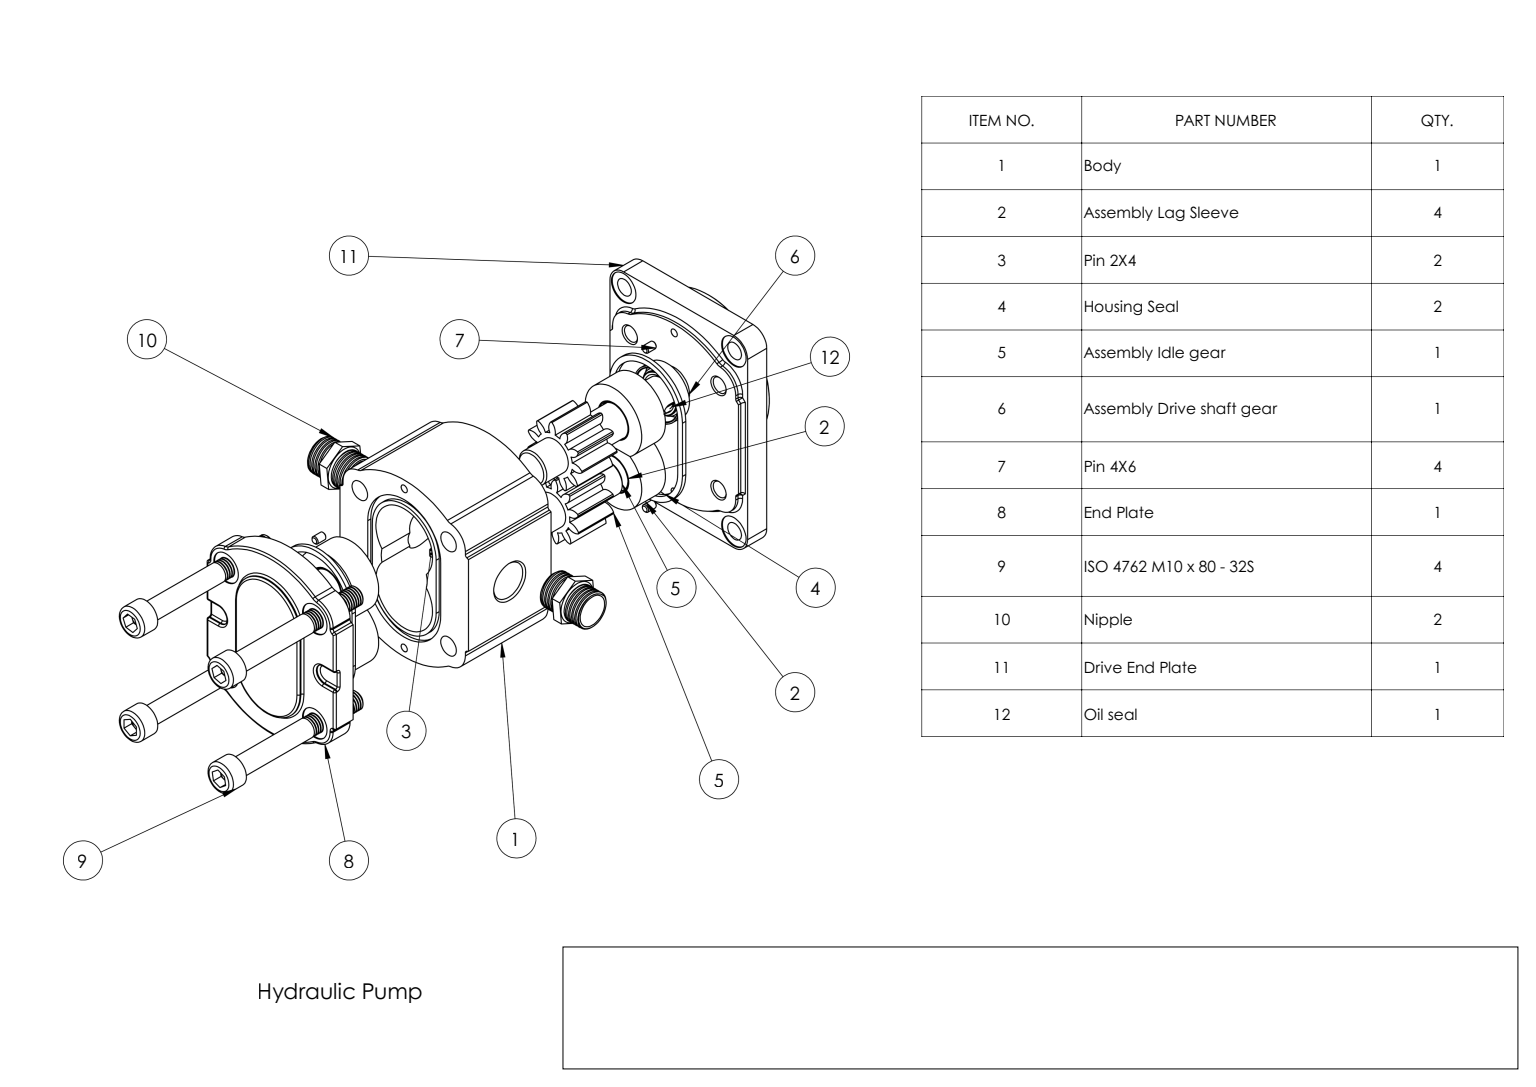
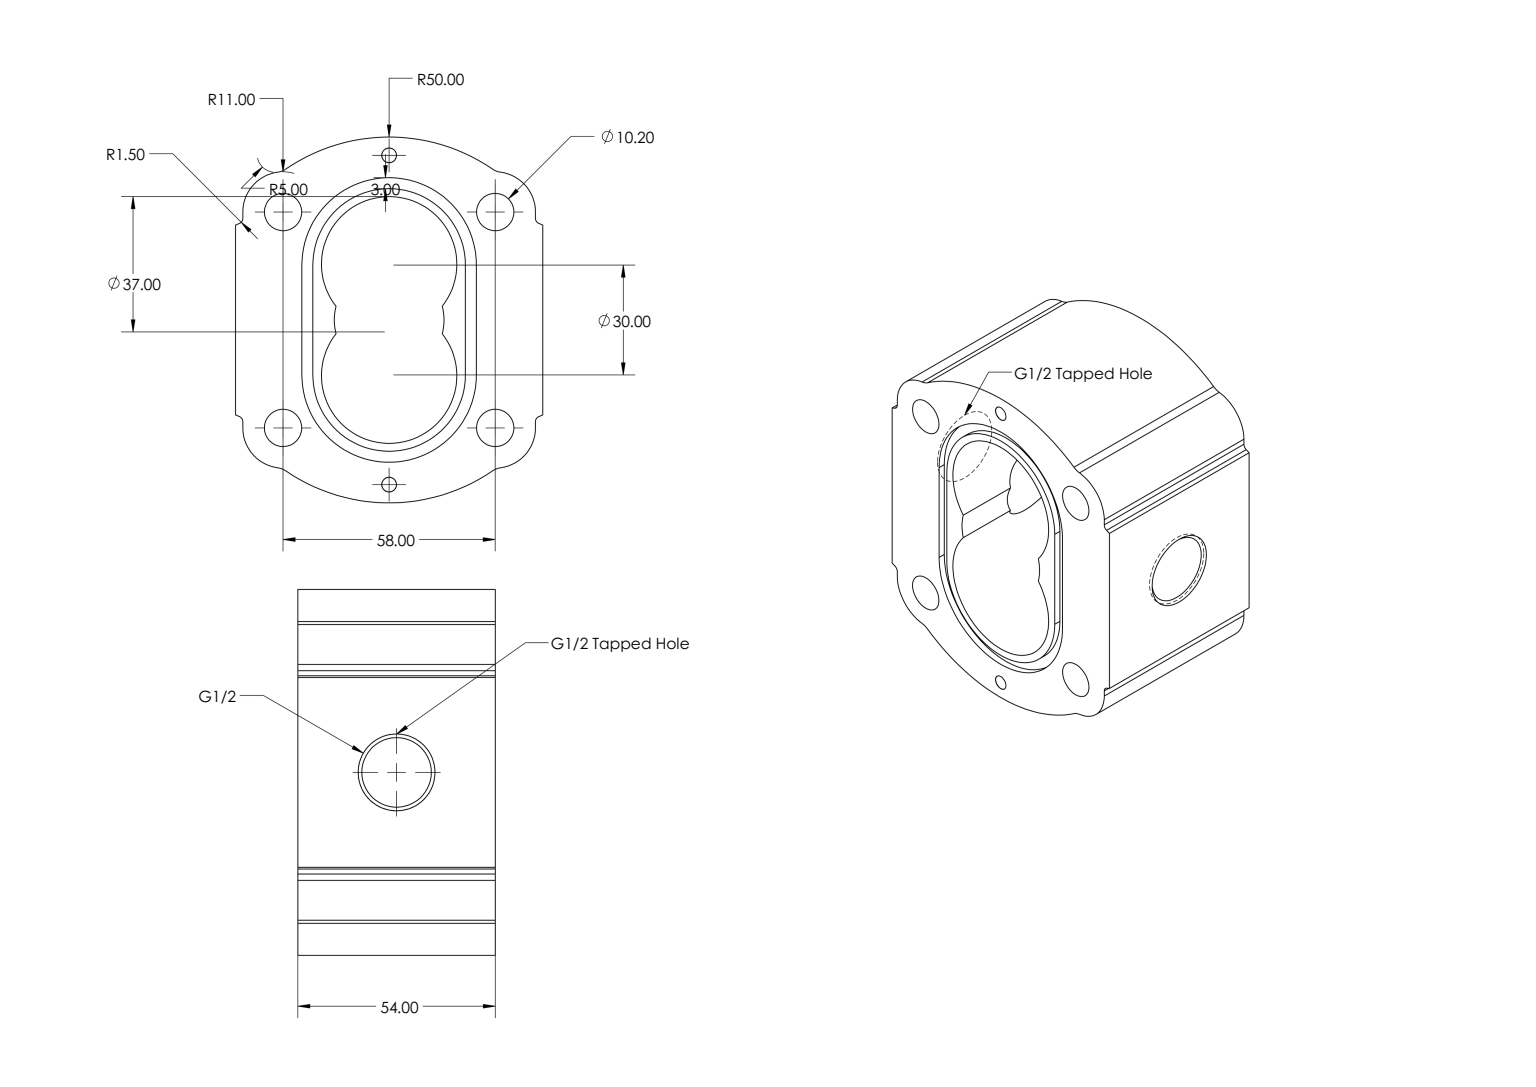
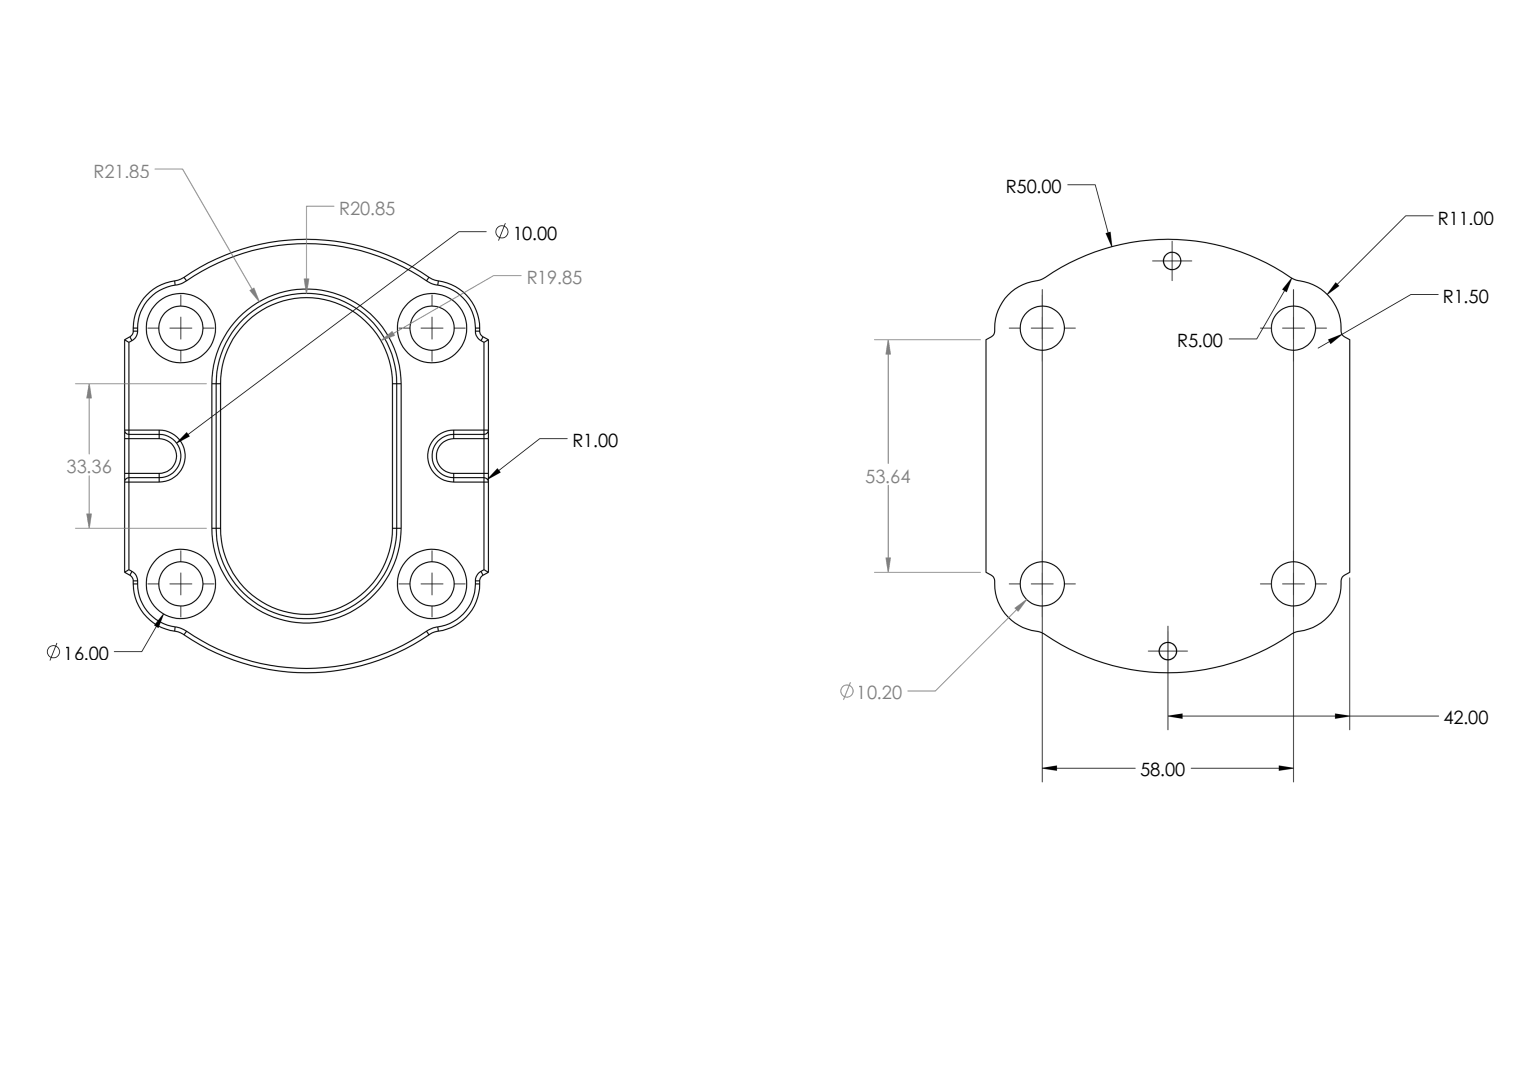
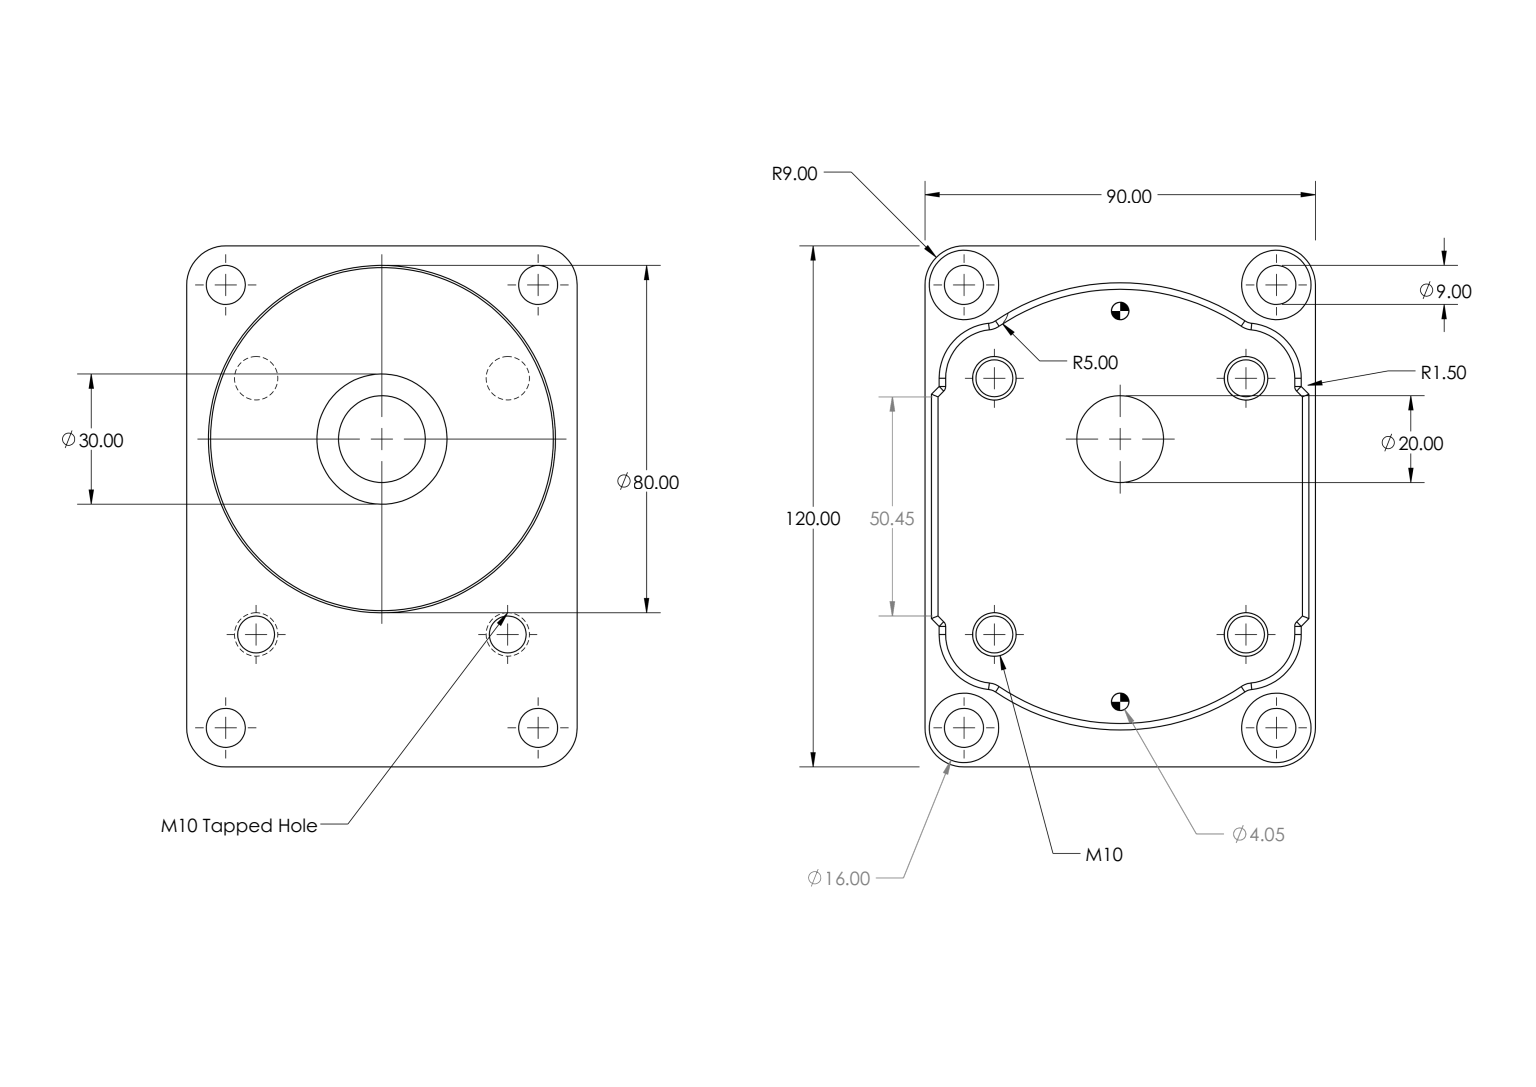
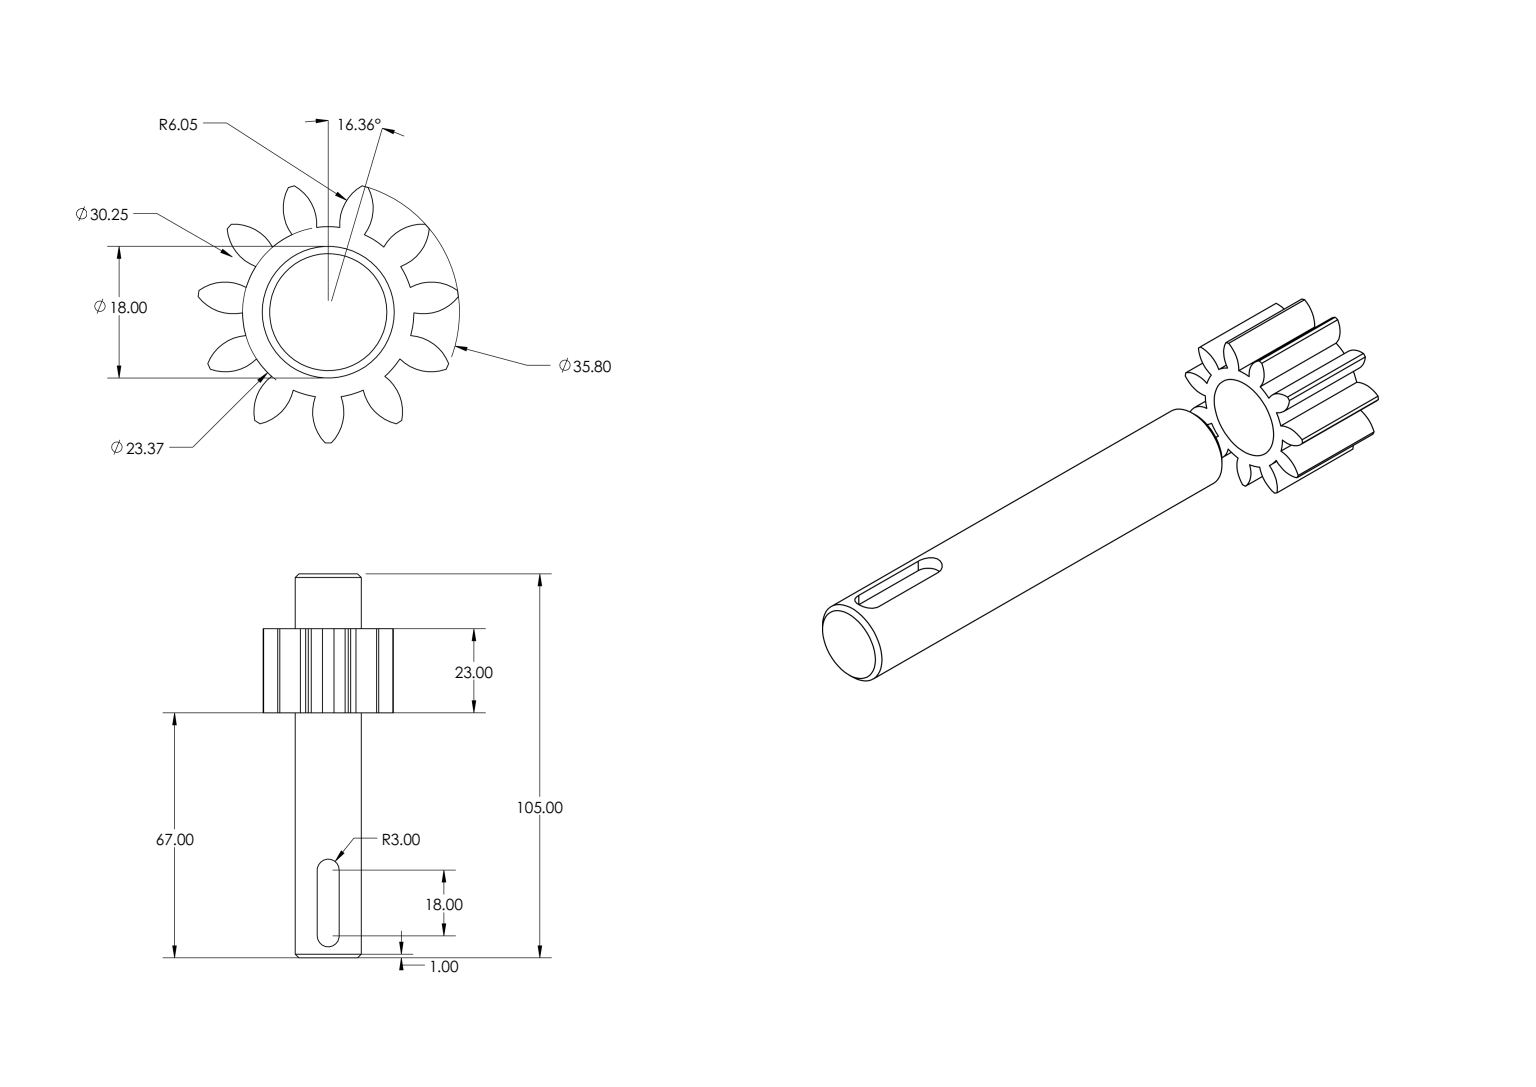
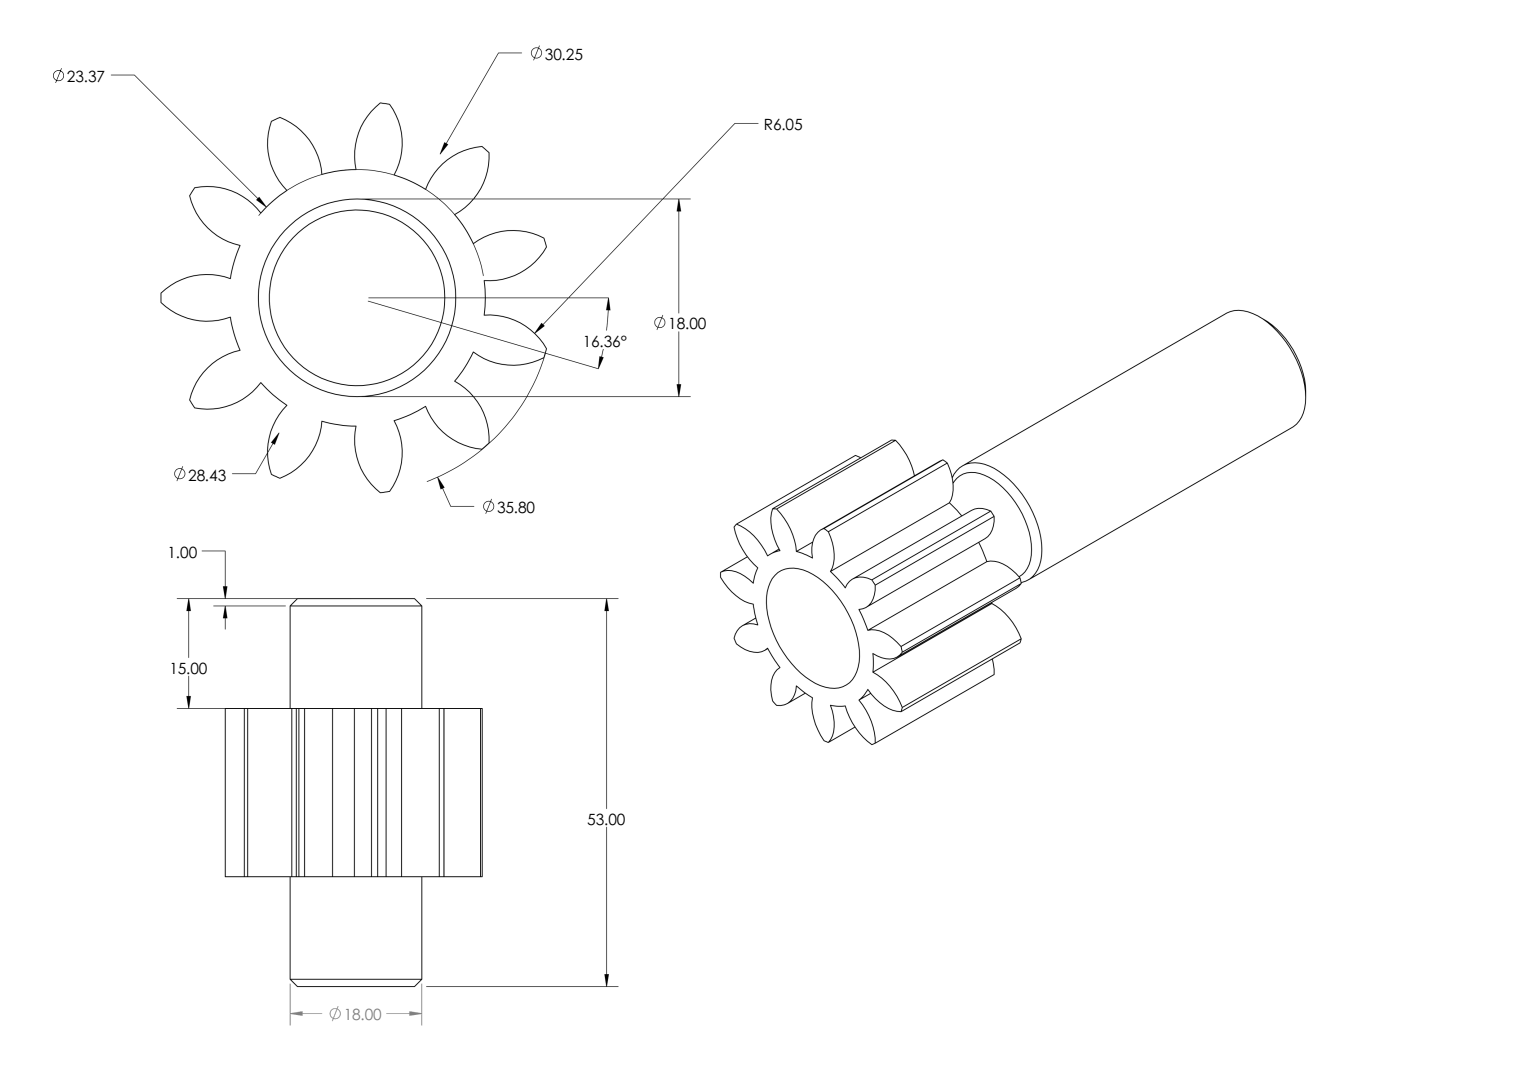
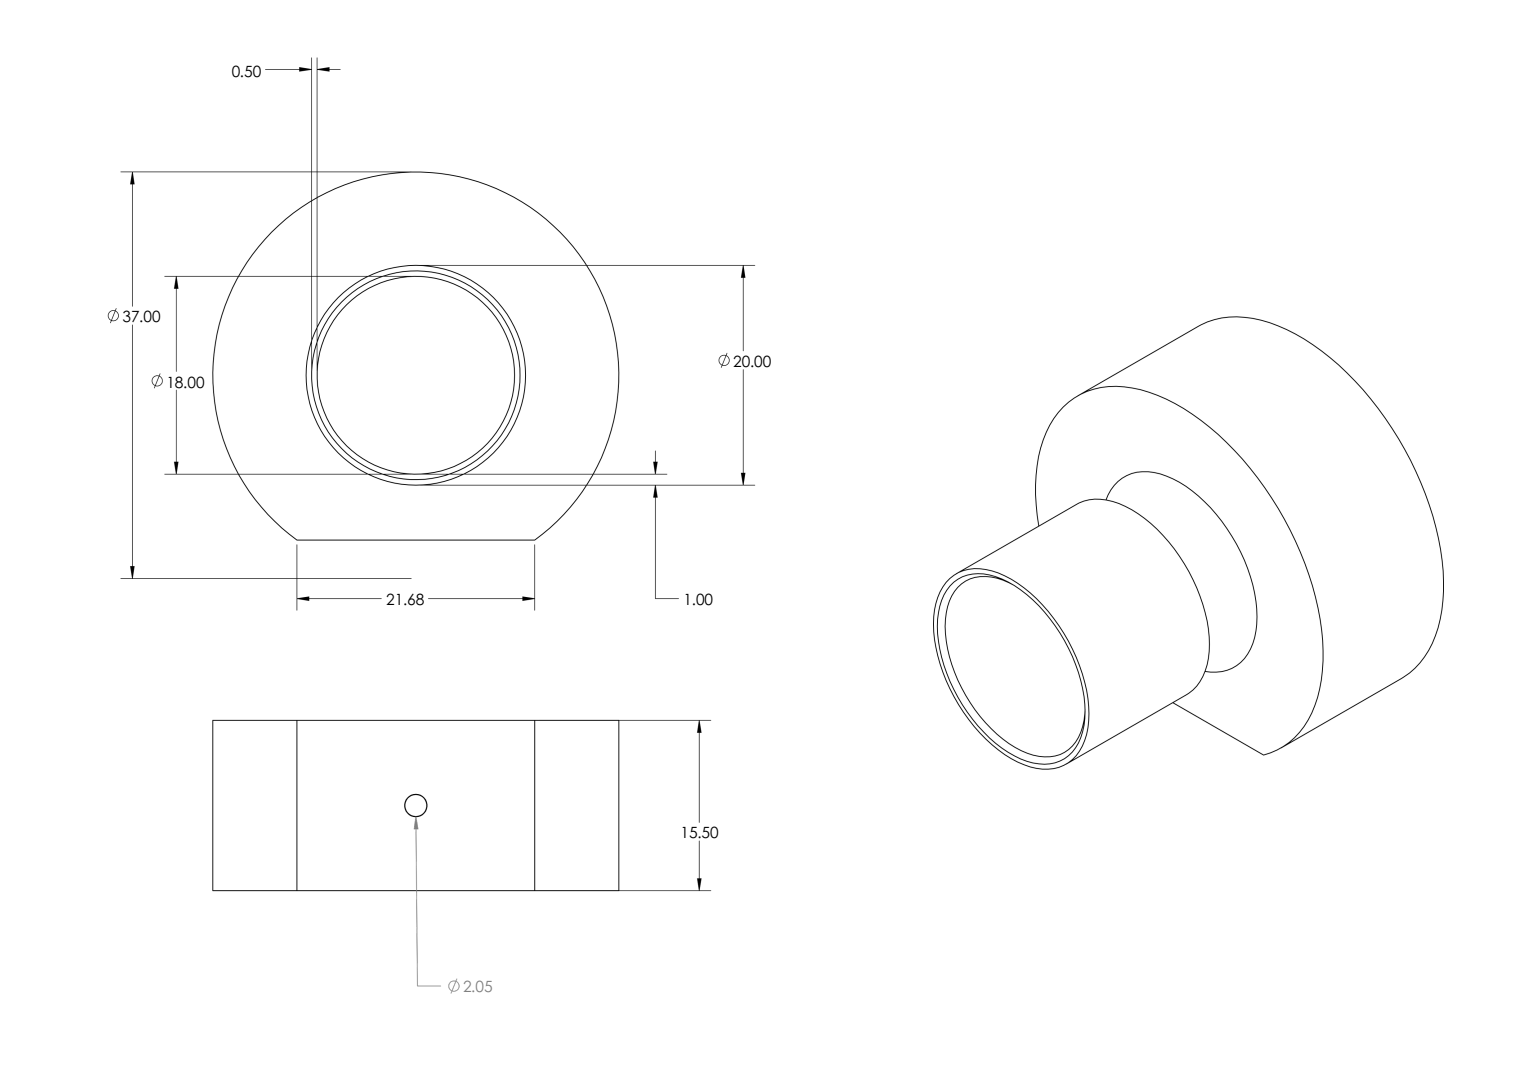
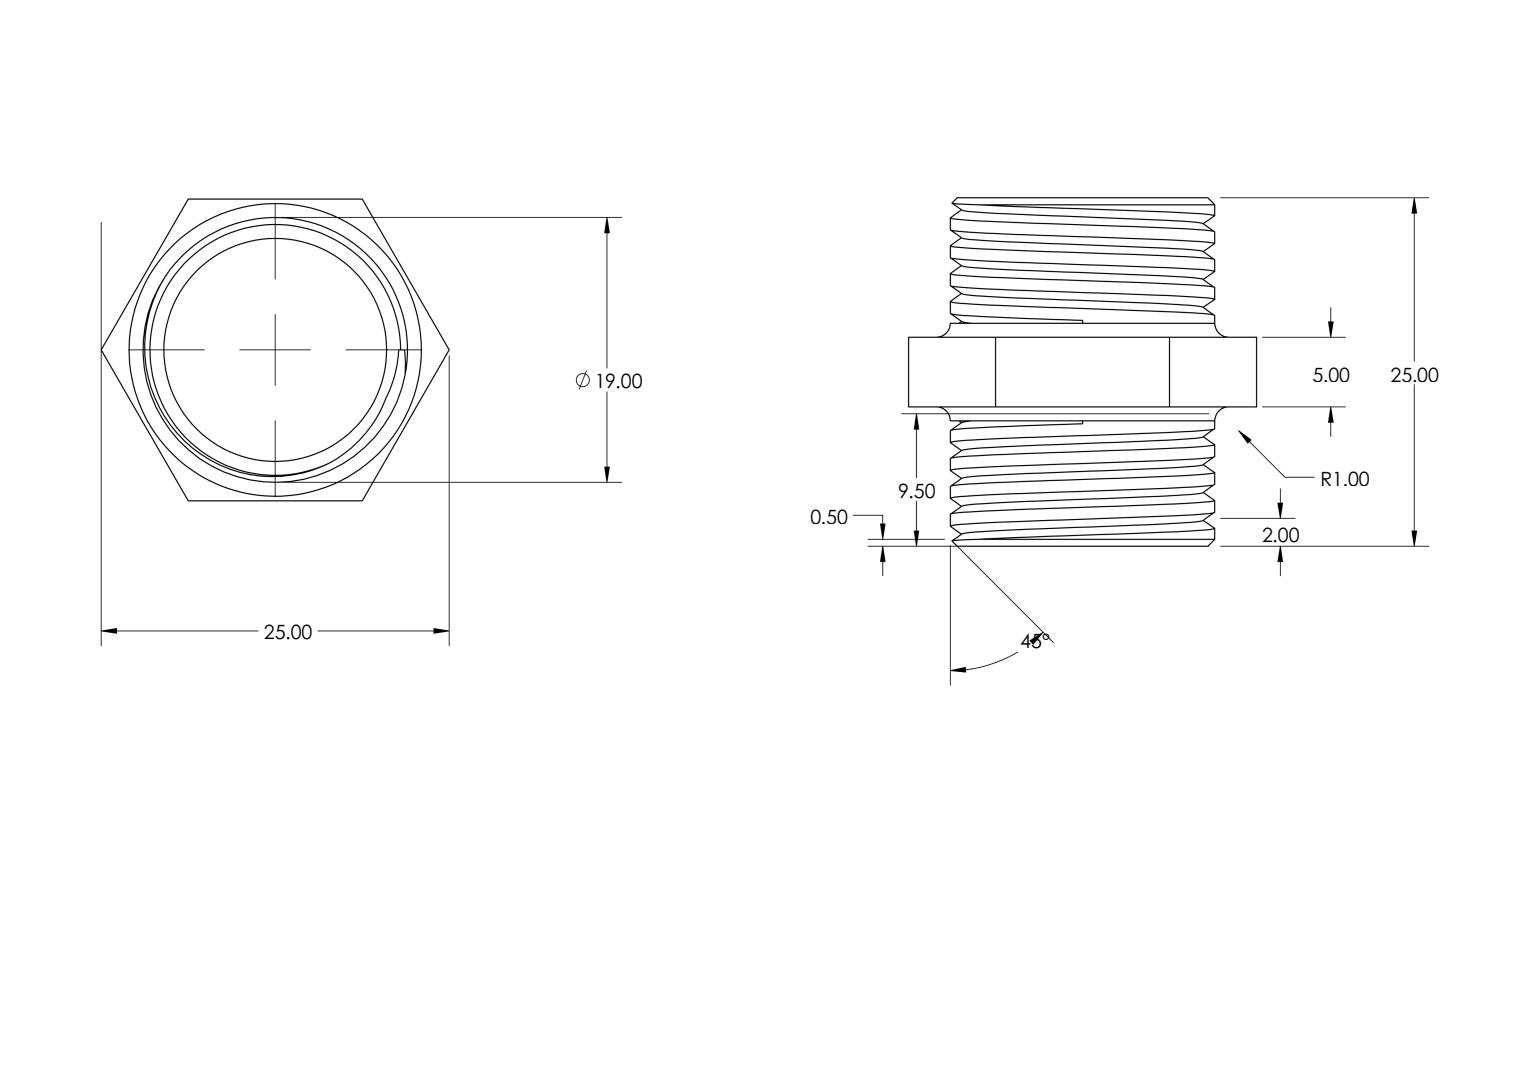
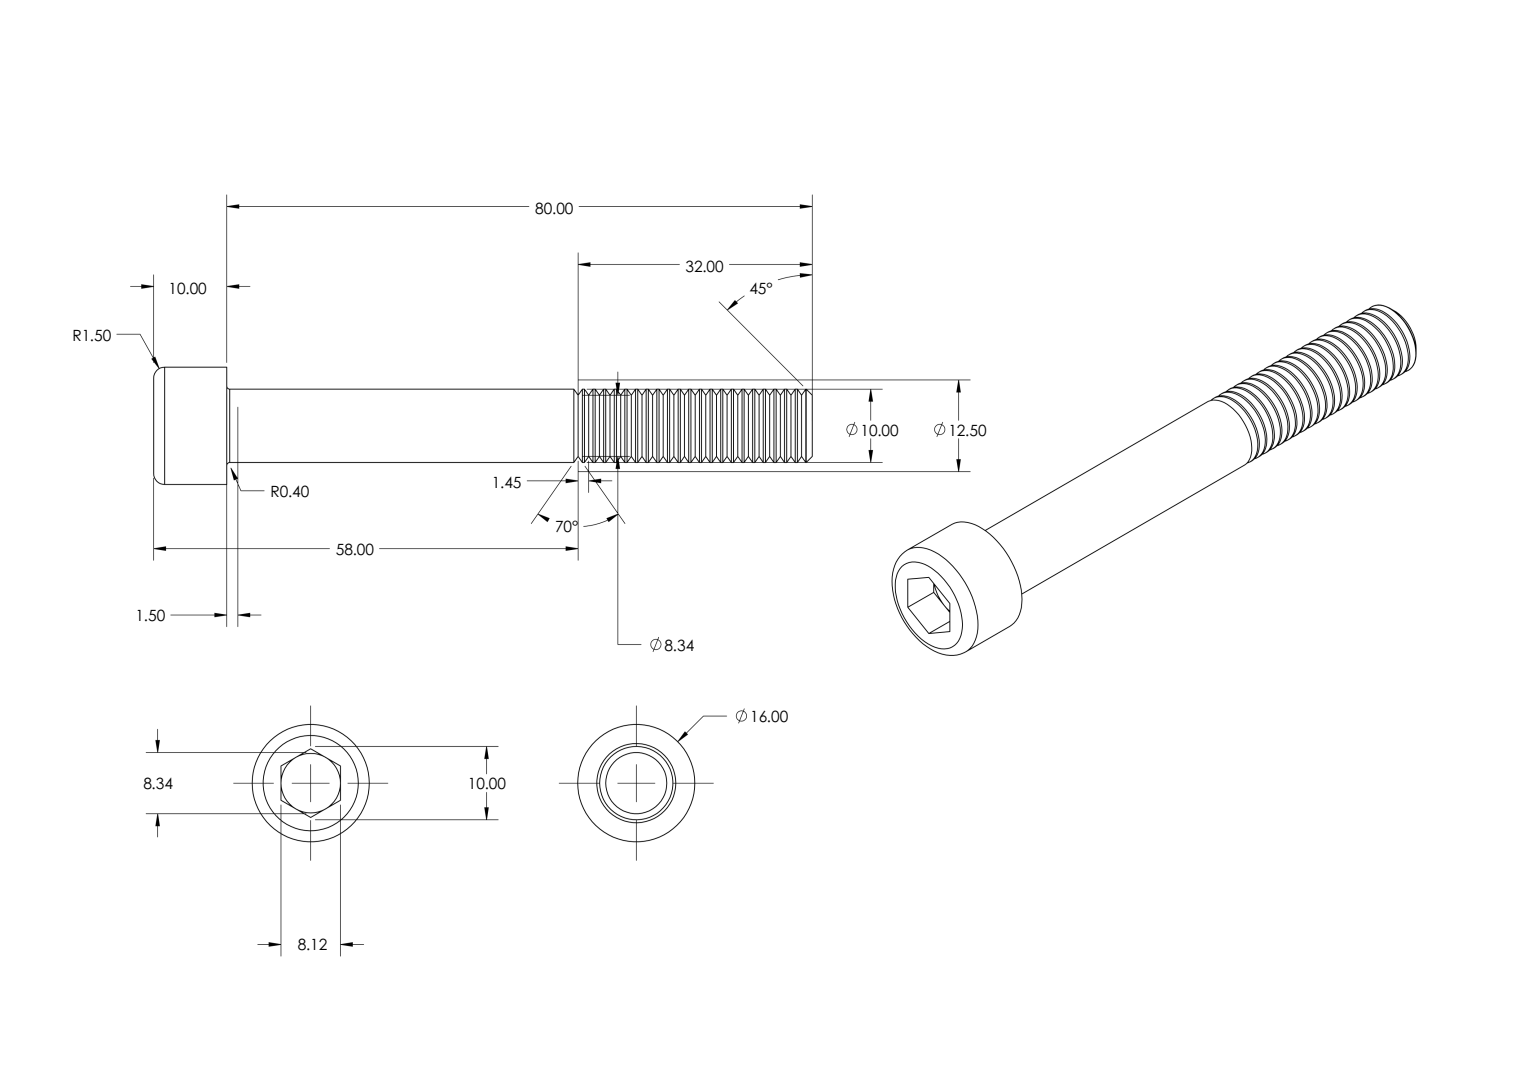
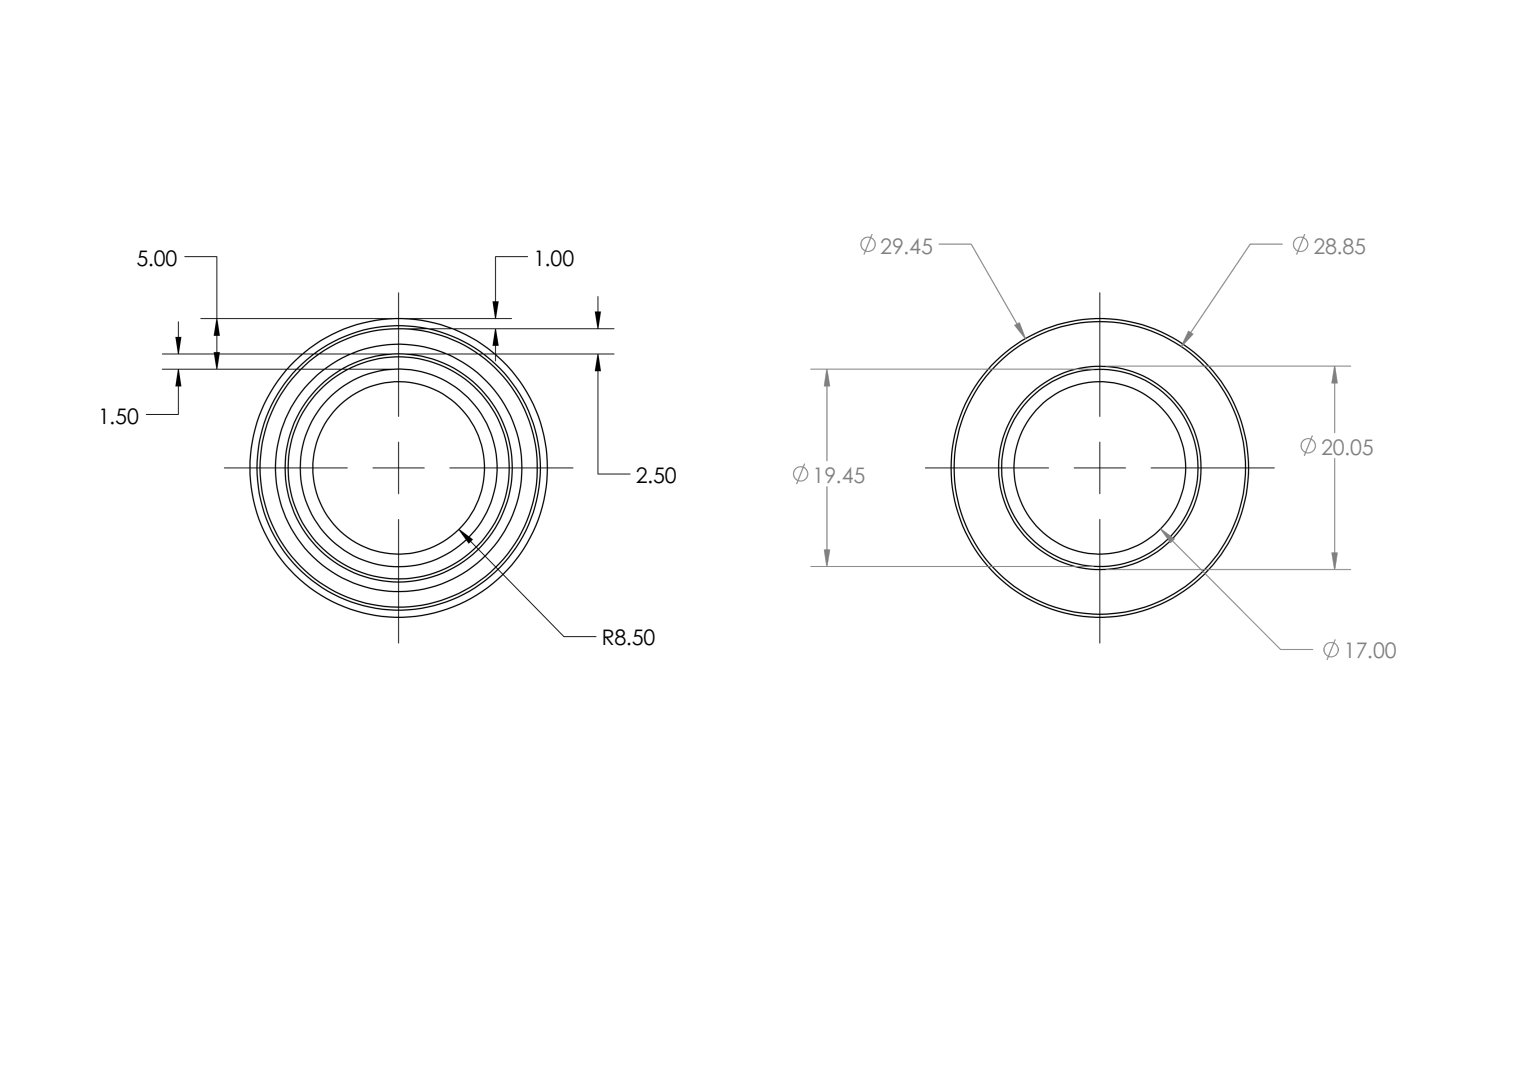
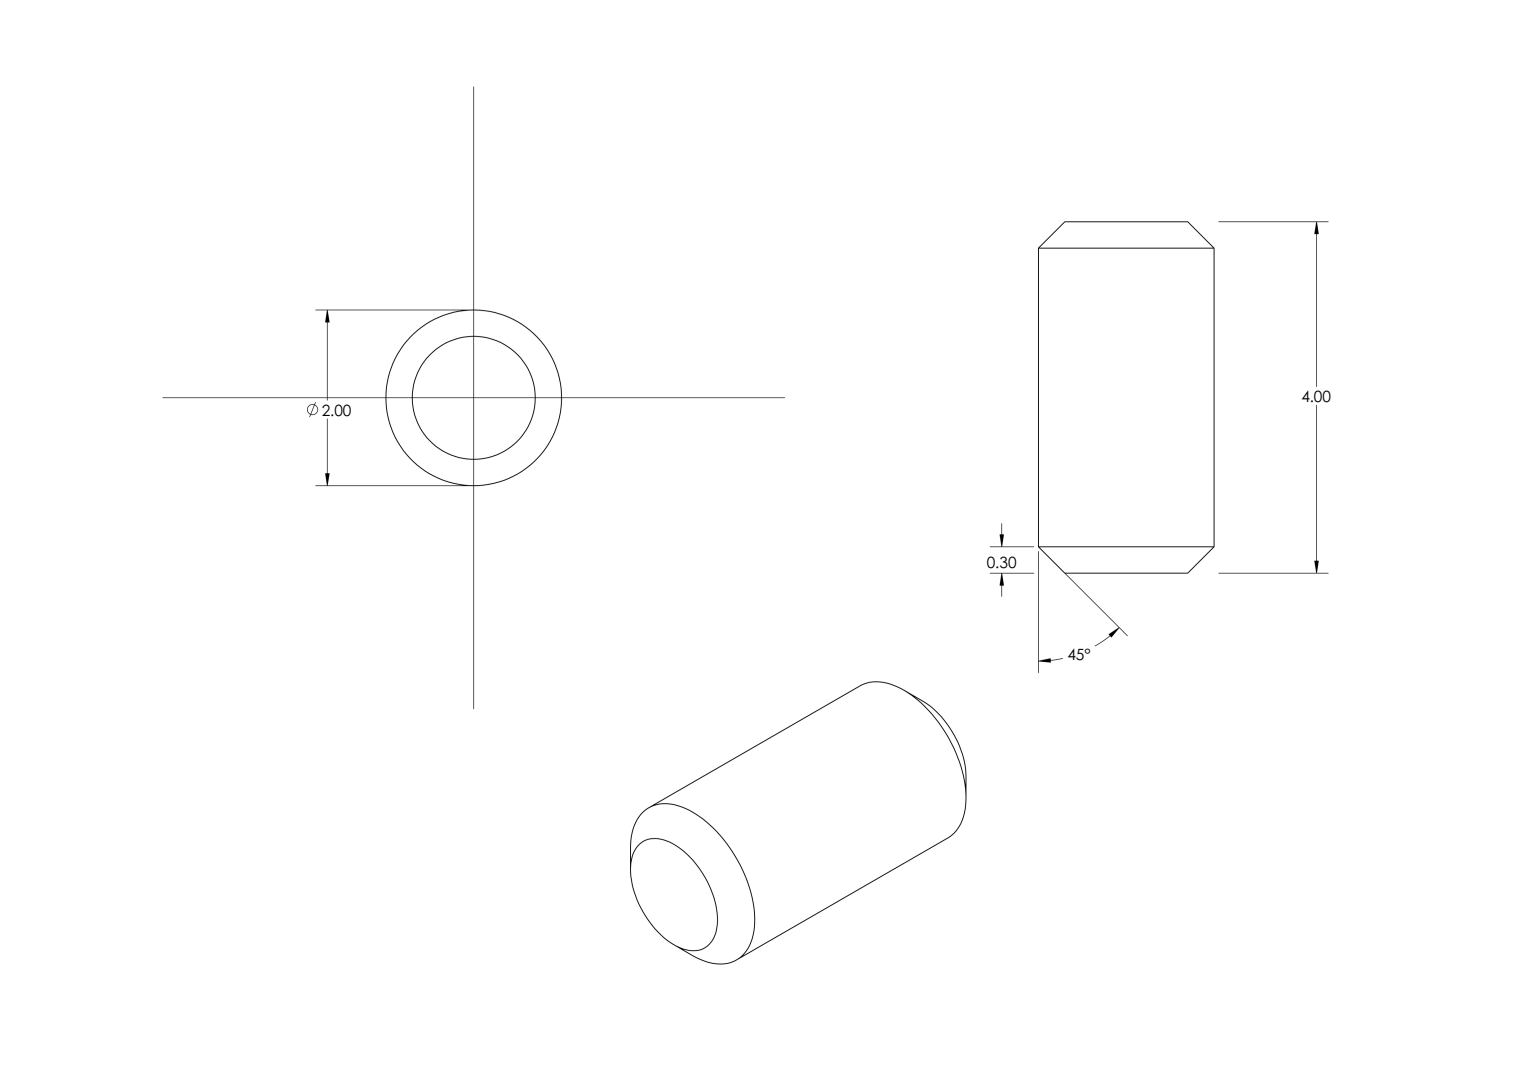
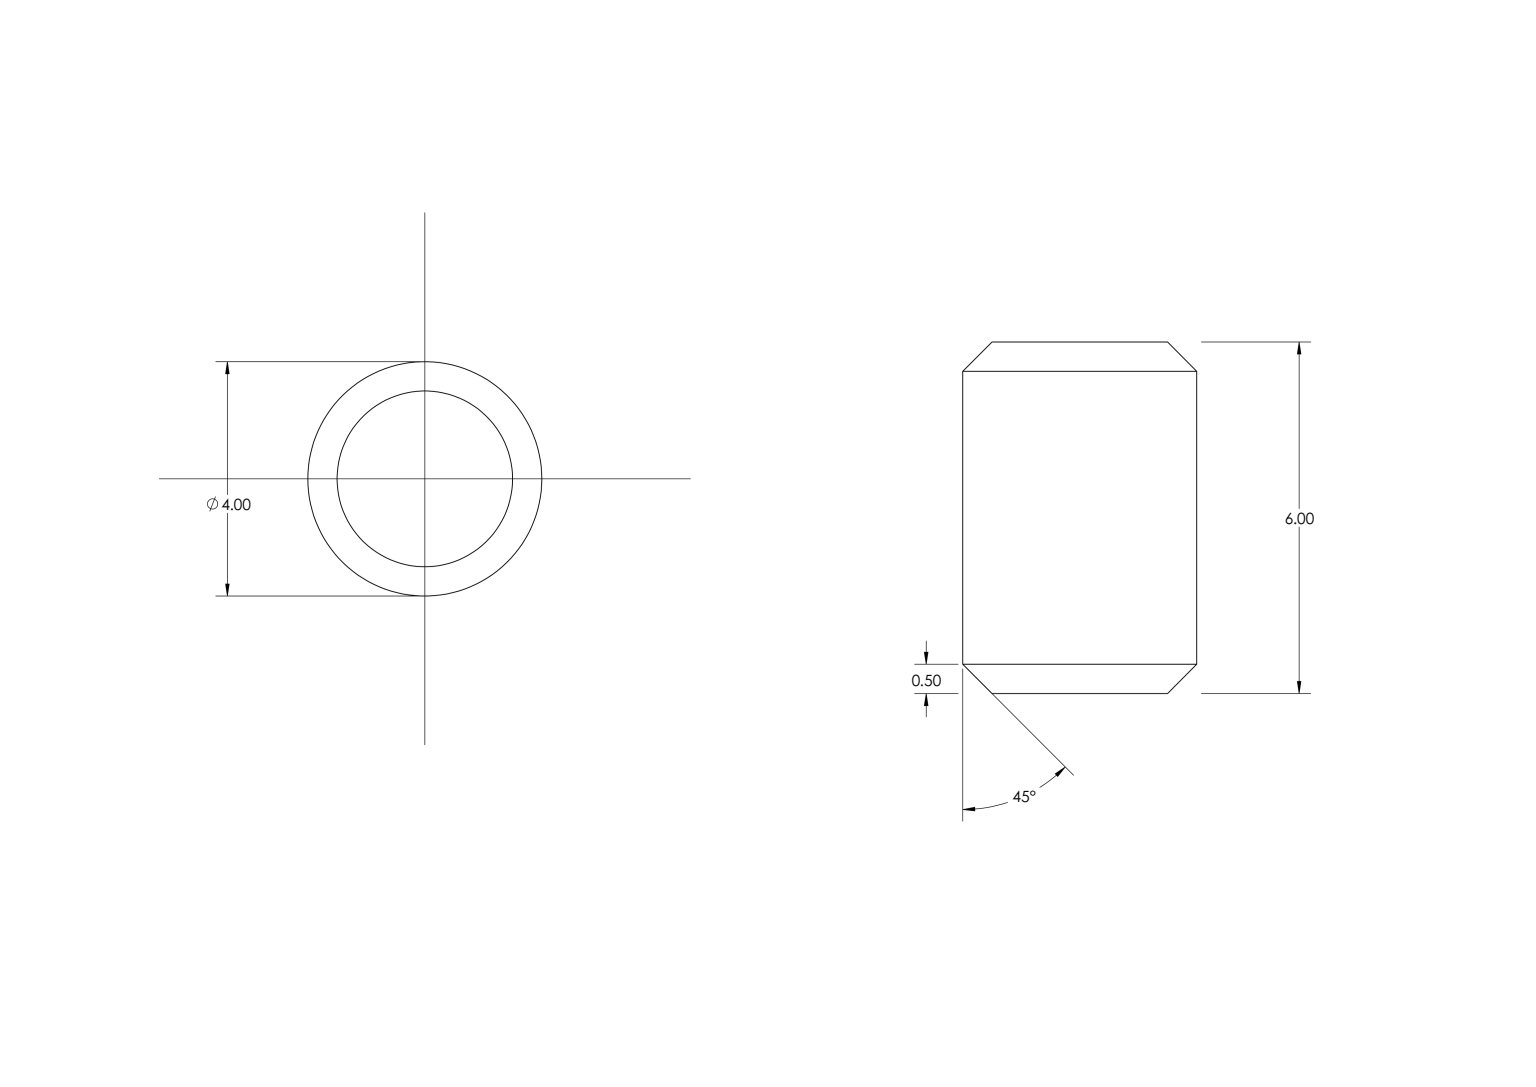
ISO-10303-21;
HEADER;
FILE_DESCRIPTION (('STEP AP214'),
    '1' );
FILE_NAME ('MAT-029',
    '2026-10-22T18:53:08',
    ( '' ),
    ( '' ),
    'SwSTEP 2.0',
    'SolidWorks 2025',
    '' );
FILE_SCHEMA (( 'AUTOMOTIVE_DESIGN' ));
ENDSEC;

DATA;
#1 = EDGE_CURVE ( 'NONE', #11499, #20840, #16615, .T. ) ;
#2 = DIRECTION ( 'NONE',  ( -0.000000000000000000, -0.000000000000000000, -1.000000000000000000 ) ) ;
#3 = ORIENTED_EDGE ( 'NONE', *, *, #12313, .F. ) ;
#4 = CARTESIAN_POINT ( 'NONE',  ( 76.90909090909090651, 4.172000000000015696, 5.109226446042767468E-16 ) ) ;
#5 = PRESENTATION_STYLE_ASSIGNMENT (( #18302 ) ) ;
#6 = DIRECTION ( 'NONE',  ( -0.000000000000000000, -0.000000000000000000, -1.000000000000000000 ) ) ;
#7 = DIRECTION ( 'NONE',  ( -1.000000000000000000, -1.224606353822377258E-16, -0.000000000000000000 ) ) ;
#8 = FACE_OUTER_BOUND ( 'NONE', #14031, .T. ) ;
#9 = DIRECTION ( 'NONE',  ( -1.000000000000000000, 0.000000000000000000, 0.000000000000000000 ) ) ;
#10 = CARTESIAN_POINT ( 'NONE',  ( -5.365059087798939252, -7.384370330707086261, -9.933165578109189653 ) ) ;
#11 = CIRCLE ( 'NONE', #13975, 5.000000000000007994 ) ;
#12 = ORIENTED_EDGE ( 'NONE', *, *, #15292, .F. ) ;
#13 = DIRECTION ( 'NONE',  ( -1.000000000000000000, -0.000000000000000000, -0.000000000000000000 ) ) ;
#14 = VERTEX_POINT ( 'NONE', #7795 ) ;
#15 = CIRCLE ( 'NONE', #8560, 2.000000000000000000 ) ;
#16 = DIRECTION ( 'NONE',  ( 1.000000000000000000, 0.000000000000000000, 0.000000000000000000 ) ) ;
#17 = EDGE_CURVE ( 'NONE', #19080, #8629, #10061, .T. ) ;
#18 = ORIENTED_EDGE ( 'NONE', *, *, #10304, .F. ) ;
#19 =( LENGTH_UNIT ( ) NAMED_UNIT ( * ) SI_UNIT ( .MILLI., .METRE. ) );
#20 = LINE ( 'NONE', #16953, #20756 ) ;
#21 = EDGE_CURVE ( 'NONE', #19190, #16784, #8531, .T. ) ;
#22 = CARTESIAN_POINT ( 'NONE',  ( 33.99999999999998579, -6.000000000000013323, 12.00000000000000000 ) ) ;
#23 = LINE ( 'NONE', #14874, #8703 ) ;
#24 = CARTESIAN_POINT ( 'NONE',  ( 2.935661446562616295, -9.035036904803758873, -7.659589141758144315 ) ) ;
#25 = VERTEX_POINT ( 'NONE', #15375 ) ;
#26 = ORIENTED_EDGE ( 'NONE', *, *, #6186, .T. ) ;
#27 = CARTESIAN_POINT ( 'NONE',  ( -31.10231664966676846, 45.36128193761570770, 11.00000000000000000 ) ) ;
#28 = VECTOR ( 'NONE', #2460, 1000.000000000000000 ) ;
#29 = ORIENTED_EDGE ( 'NONE', *, *, #14693, .F. ) ;
#30 = ORIENTED_EDGE ( 'NONE', *, *, #13409, .T. ) ;
#31 = FACE_OUTER_BOUND ( 'NONE', #11756, .T. ) ;
#32 = CYLINDRICAL_SURFACE ( 'NONE', #17288, 5.000000000000000888 ) ;
#33 = DIRECTION ( 'NONE',  ( 1.000000000000000000, 0.000000000000000000, 0.000000000000000000 ) ) ;
#34 = ORIENTED_EDGE ( 'NONE', *, *, #12812, .F. ) ;
#35 = CARTESIAN_POINT ( 'NONE',  ( -6.021009868636381950E-13, 9.295211988927752245, 2.702983250845903740 ) ) ;
#36 = DIRECTION ( 'NONE',  ( 0.000000000000000000, 0.000000000000000000, 1.000000000000000000 ) ) ;
#37 = CARTESIAN_POINT ( 'NONE',  ( 73.42022815836234884, 7.420530141404717394E-15, 0.000000000000000000 ) ) ;
#38 = DIRECTION ( 'NONE',  ( -0.4828336235133057208, -0.8757121056631633760, 0.000000000000000000 ) ) ;
#39 = CARTESIAN_POINT ( 'NONE',  ( 8.680847955710813579, 2.820578480814259326, 4.733165578109188587 ) ) ;
#40 = AXIS2_PLACEMENT_3D ( 'NONE', #5104, #5351, #18285 ) ;
#41 = ORIENTED_EDGE ( 'NONE', *, *, #8594, .T. ) ;
#42 = EDGE_CURVE ( 'NONE', #9946, #3596, #16307, .T. ) ;
#43 = PRODUCT ( 'Part10^Assembly Drive shaft gear', 'Part10^Assembly Drive shaft gear', '', ( #22523 ) ) ;
#44 = ORIENTED_EDGE ( 'NONE', *, *, #15427, .T. ) ;
#45 = ADVANCED_FACE ( 'NONE', ( #13562 ), #20757, .T. ) ;
#46 = ORIENTED_EDGE ( 'NONE', *, *, #10714, .T. ) ;
#47 = VERTEX_POINT ( 'NONE', #16968 ) ;
#48 = ITEM_DEFINED_TRANSFORMATION ( 'NONE', 'NONE', #5314,  #8005 ) ;
#49 = EDGE_LOOP ( 'NONE', ( #12692, #15441, #20790, #14111 ) ) ;
#50 = FACE_OUTER_BOUND ( 'NONE', #14923, .T. ) ;
#51 = CARTESIAN_POINT ( 'NONE',  ( 23.00000000000000000, 10.59264252385236738, 4.936618945406631376 ) ) ;
#52 = ORIENTED_EDGE ( 'NONE', *, *, #5845, .F. ) ;
#53 = ORIENTED_EDGE ( 'NONE', *, *, #10449, .T. ) ;
#54 = CARTESIAN_POINT ( 'NONE',  ( 20.85000000000000497, -15.04000000000000092, 2.200000000000000178 ) ) ;
#55 = ORIENTED_EDGE ( 'NONE', *, *, #9968, .T. ) ;
#56 = CARTESIAN_POINT ( 'NONE',  ( 35.99999999999992184, -60.00000000000000000, 0.000000000000000000 ) ) ;
#57 = CIRCLE ( 'NONE', #17578, 23.85000000000000497 ) ;
#58 = CARTESIAN_POINT ( 'NONE',  ( 9.500000000000209610, -3.086737114211962396, 11.10674201446023446 ) ) ;
#59 = PRODUCT_RELATED_PRODUCT_CATEGORY ( 'part', '', ( #10410 ) ) ;
#60 = DIRECTION ( 'NONE',  ( -0.000000000000000000, -0.000000000000000000, -1.000000000000000000 ) ) ;
#61 = VECTOR ( 'NONE', #8595, 1000.000000000000000 ) ;
#62 = CARTESIAN_POINT ( 'NONE',  ( -28.99999999999999645, -29.50000000000000000, 12.50000000000000000 ) ) ;
#63 = EDGE_CURVE ( 'NONE', #8004, #14530, #22184, .T. ) ;
#64 = DIRECTION ( 'NONE',  ( -0.000000000000000000, 0.000000000000000000, -1.000000000000000000 ) ) ;
#65 = CARTESIAN_POINT ( 'NONE',  ( 1.499999999999998668, 0.000000000000000000, 0.000000000000000000 ) ) ;
#66 = DIRECTION ( 'NONE',  ( 1.000000000000000000, 0.000000000000000000, -0.000000000000000000 ) ) ;
#67 = DIRECTION ( 'NONE',  ( -1.000000000000000000, -0.000000000000000000, -0.000000000000000000 ) ) ;
#68 = ORIENTED_EDGE ( 'NONE', *, *, #149, .T. ) ;
#69 = EDGE_CURVE ( 'NONE', #19085, #18693, #18803, .T. ) ;
#70 = ORIENTED_EDGE ( 'NONE', *, *, #15637, .T. ) ;
#71 = CARTESIAN_POINT ( 'NONE',  ( -8.680847955711007202, -5.923547351154968927E-13, 7.633165578109188942 ) ) ;
#72 = ORIENTED_EDGE ( 'NONE', *, *, #21290, .F. ) ;
#73 = ADVANCED_FACE ( 'NONE', ( #6232 ), #15009, .T. ) ;
#74 = EDGE_CURVE ( 'NONE', #21063, #2169, #4296, .T. ) ;
#75 = APPLICATION_PROTOCOL_DEFINITION ( 'draft international standard', 'automotive_design', 1998, #10704 ) ;
#76 = TOROIDAL_SURFACE ( 'NONE', #15632, 14.42592346043842433, 0.2999999999999999334 ) ;
#77 = ORIENTED_EDGE ( 'NONE', *, *, #3083, .F. ) ;
#78 = ORIENTED_EDGE ( 'NONE', *, *, #6210, .T. ) ;
#79 = LINE ( 'NONE', #7484, #19699 ) ;
#80 = CARTESIAN_POINT ( 'NONE',  ( 7.022953521755574080, -5.102474405759714671, -8.433165578109187877 ) ) ;
#81 = AXIS2_PLACEMENT_3D ( 'NONE', #23504, #16172, #14329 ) ;
#82 = CARTESIAN_POINT ( 'NONE',  ( 5.000000000000000000, 2.342598717236902939, -4.057500000000001883 ) ) ;
#83 = EDGE_LOOP ( 'NONE', ( #14204, #20544 ) ) ;
#84 = LINE ( 'NONE', #7029, #8324 ) ;
#85 = CARTESIAN_POINT ( 'NONE',  ( 0.000000000000000000, 6.242160243097161221, 9.879763041175145588 ) ) ;
#86 = DIRECTION ( 'NONE',  ( 1.000000000000000000, 0.000000000000000000, 0.000000000000000000 ) ) ;
#87 = DIRECTION ( 'NONE',  ( 1.000000000000000000, 0.000000000000000000, 0.000000000000000000 ) ) ;
#88 = ORIENTED_EDGE ( 'NONE', *, *, #16385, .T. ) ;
#89 = DIRECTION ( 'NONE',  ( -1.000000000000000000, -0.000000000000000000, 0.000000000000000000 ) ) ;
#90 = ORIENTED_EDGE ( 'NONE', *, *, #11501, .F. ) ;
#91 = ORIENTED_EDGE ( 'NONE', *, *, #20484, .F. ) ;
#92 = CARTESIAN_POINT ( 'NONE',  ( 9.500000000000000000, 1.163414459189985485E-15, 11.99999999999999645 ) ) ;
#93 = CARTESIAN_POINT ( 'NONE',  ( -6.822232771736904647E-13, 9.988891130263535700, -8.559589141758142006 ) ) ;
#94 = CARTESIAN_POINT ( 'NONE',  ( 3.530011532367169913, 0.000000000000000000, 11.23654394515110511 ) ) ;
#95 = CARTESIAN_POINT ( 'NONE',  ( 20.85000000000000497, -16.67999999999999616, 13.00000000000000178 ) ) ;
#96 = EDGE_CURVE ( 'NONE', #2943, #5490, #6588, .T. ) ;
#97 = CIRCLE ( 'NONE', #7457, 5.000000000000007994 ) ;
#98 = AXIS2_PLACEMENT_3D ( 'NONE', #4518, #4374, #19265 ) ;
#99 = FACE_OUTER_BOUND ( 'NONE', #13945, .T. ) ;
#100 = CARTESIAN_POINT ( 'NONE',  ( 2.682529543900284974, -8.255977015246234174, -12.23316557810919036 ) ) ;
#101 = VECTOR ( 'NONE', #13644, 1000.000000000000000 ) ;
#102 = AXIS2_PLACEMENT_3D ( 'NONE', #2204, #20880, #21238 ) ;
#103 = AXIS2_PLACEMENT_3D ( 'NONE', #19821, #17978, #17736 ) ;
#104 =( NAMED_UNIT ( * ) PLANE_ANGLE_UNIT ( ) SI_UNIT ( $, .RADIAN. ) );
#105 = VERTEX_POINT ( 'NONE', #507 ) ;
#106 = ORIENTED_EDGE ( 'NONE', *, *, #4031, .T. ) ;
#107 = VECTOR ( 'NONE', #16145, 1000.000000000000000 ) ;
#108 = EDGE_CURVE ( 'NONE', #8629, #11642, #11625, .T. ) ;
#109 = ORIENTED_EDGE ( 'NONE', *, *, #14382, .F. ) ;
#110 = ADVANCED_FACE ( 'NONE', ( #6119 ), #2088, .T. ) ;
#111 = ORIENTED_EDGE ( 'NONE', *, *, #20184, .F. ) ;
#112 = DIRECTION ( 'NONE',  ( -0.000000000000000000, -0.000000000000000000, -1.000000000000000000 ) ) ;
#113 = CARTESIAN_POINT ( 'NONE',  ( -23.84999999999999432, -15.03999999999999915, 27.00000000000000000 ) ) ;
#114 = CONICAL_SURFACE ( 'NONE', #9806, 5.000000000000007994, 0.9599310885968855844 ) ;
#115 = CARTESIAN_POINT ( 'NONE',  ( -42.00000000000000000, -6.000000000000000888, 12.00000000000000000 ) ) ;
#116 = LINE ( 'NONE', #7524, #12182 ) ;
#117 = CIRCLE ( 'NONE', #3217, 5.099999999999996980 ) ;
#118 = AXIS2_PLACEMENT_3D ( 'NONE', #19032, #3780, #14981 ) ;
#119 = VECTOR ( 'NONE', #13180, 1000.000000000000000 ) ;
#120 = EDGE_LOOP ( 'NONE', ( #21996, #2692, #5387 ) ) ;
#121 = AXIS2_PLACEMENT_3D ( 'NONE', #7421, #9361, #16 ) ;
#122 = FACE_OUTER_BOUND ( 'NONE', #9649, .T. ) ;
#123 = FACE_OUTER_BOUND ( 'NONE', #13538, .T. ) ;
#124 = CARTESIAN_POINT ( 'NONE',  ( -17.32314925601269451, 8.733074366907754182, 3.769949228126193930 ) ) ;
#125 = LINE ( 'NONE', #22458, #18476 ) ;
#126 = ORIENTED_EDGE ( 'NONE', *, *, #5435, .F. ) ;
#127 = CYLINDRICAL_SURFACE ( 'NONE', #11099, 4.999999999999997335 ) ;
#128 = VERTEX_POINT ( 'NONE', #9516 ) ;
#129 = CARTESIAN_POINT ( 'NONE',  ( -14.99999999999999822, 0.000000000000000000, 27.00000000000000000 ) ) ;
#130 = ORIENTED_EDGE ( 'NONE', *, *, #3083, .T. ) ;
#132 = VECTOR ( 'NONE', #9378, 999.9999999999998863 ) ;
#131 = B_SPLINE_CURVE_WITH_KNOTS ( 'NONE', 3,
 ( #17555, #9865, #6107, #23059, #11576, #21099, #8039, #15483, #7911, #6478, #12055, #17073, #5983, #17321 ),
 .UNSPECIFIED., .F., .F.,
 ( 4, 2, 2, 2, 2, 2, 4 ),
 ( 6.929308356866153103E-16, 0.001553140985941692384, 0.002329711478912192824, 0.003106281971882693047, 0.004659422957823693492, 0.005435993450794191981, 0.006212563943764690469 ),
 .UNSPECIFIED. ) ;
#133 = CARTESIAN_POINT ( 'NONE',  ( 7.685661446562381371, -5.583959896777971110, -9.859589141758144493 ) ) ;
#134 = AXIS2_PLACEMENT_3D ( 'NONE', #7164, #10463, #7038 ) ;
#135 = EDGE_CURVE ( 'NONE', #23003, #4329, #4255, .T. ) ;
#136 = AXIS2_PLACEMENT_3D ( 'NONE', #11343, #23969, #18827 ) ;
#137 = ORIENTED_EDGE ( 'NONE', *, *, #768, .T. ) ;
#138 = CIRCLE ( 'NONE', #3244, 1.500000000000000000 ) ;
#139 = EDGE_CURVE ( 'NONE', #6140, #16103, #754, .T. ) ;
#140 = DIRECTION ( 'NONE',  ( -0.000000000000000000, -0.000000000000000000, -1.000000000000000000 ) ) ;
#141 = CIRCLE ( 'NONE', #13764, 5.000000000000007994 ) ;
#142 = CARTESIAN_POINT ( 'NONE',  ( 78.36363636363637397, 7.491529369508391930E-15, 0.000000000000000000 ) ) ;
#143 = DIRECTION ( 'NONE',  ( 0.000000000000000000, -1.000000000000000000, 0.000000000000000000 ) ) ;
#144 = CARTESIAN_POINT ( 'NONE',  ( -9.500000000000000000, -6.482511860946779655E-13, -5.059589141758143782 ) ) ;
#145 = VERTEX_POINT ( 'NONE', #9704 ) ;
#146 = DIRECTION ( 'NONE',  ( -1.000000000000000000, 0.000000000000000000, -0.000000000000000000 ) ) ;
#147 = CARTESIAN_POINT ( 'NONE',  ( -10.83999999999999986, -14.99147757894464306, 15.50000000000000000 ) ) ;
#148 = AXIS2_PLACEMENT_3D ( 'NONE', #10109, #500, #7919 ) ;
#149 = EDGE_CURVE ( 'NONE', #1960, #22892, #17041, .T. ) ;
#150 = ORIENTED_EDGE ( 'NONE', *, *, #12548, .T. ) ;
#151 = DIRECTION ( 'NONE',  ( -0.000000000000000000, -0.000000000000000000, 1.000000000000000000 ) ) ;
#152 = AXIS2_PLACEMENT_3D ( 'NONE', #5788, #7824, #2121 ) ;
#153 = AXIS2_PLACEMENT_3D ( 'NONE', #4765, #13942, #9753 ) ;
#154 = CIRCLE ( 'NONE', #18789, 5.000000000000007994 ) ;
#155 = EDGE_CURVE ( 'NONE', #21886, #19378, #14378, .T. ) ;
#156 = AXIS2_PLACEMENT_3D ( 'NONE', #18360, #1648, #3839 ) ;
#157 = DIRECTION ( 'NONE',  ( -1.000000000000000000, -0.000000000000000000, -0.000000000000000000 ) ) ;
#158 = AXIS2_PLACEMENT_3D ( 'NONE', #9827, #13523, #460 ) ;
#159 = DIRECTION ( 'NONE',  ( -1.000000000000000000, 0.000000000000000000, 0.000000000000000000 ) ) ;
#160 = FACE_OUTER_BOUND ( 'NONE', #18742, .T. ) ;
#161 = DIRECTION ( 'NONE',  ( 0.000000000000000000, -1.000000000000000000, 0.000000000000000000 ) ) ;
#162 = ORIENTED_EDGE ( 'NONE', *, *, #164, .T. ) ;
#163 = DIRECTION ( 'NONE',  ( -0.000000000000000000, -0.000000000000000000, -1.000000000000000000 ) ) ;
#164 = EDGE_CURVE ( 'NONE', #8624, #9243, #17159, .T. ) ;
#165 = CYLINDRICAL_SURFACE ( 'NONE', #16449, 23.85000000000000142 ) ;
#166 = EDGE_CURVE ( 'NONE', #9633, #17850, #16710, .T. ) ;
#167 = DIRECTION ( 'NONE',  ( 1.000000000000000000, 0.000000000000000000, 0.000000000000000000 ) ) ;
#168 = DIRECTION ( 'NONE',  ( -0.7089874389501492624, -0.7052211081716913688, 0.000000000000000000 ) ) ;
#169 = ORIENTED_EDGE ( 'NONE', *, *, #19806, .T. ) ;
#170 = ORIENTED_EDGE ( 'NONE', *, *, #21885, .F. ) ;
#171 = CIRCLE ( 'NONE', #23551, 8.000000000000003553 ) ;
#172 = CONTEXT_DEPENDENT_SHAPE_REPRESENTATION ( #5586, #1080 ) ;
#174 = ORIENTED_EDGE ( 'NONE', *, *, #5150, .T. ) ;
#173 = VECTOR ( 'NONE', #911, 1000.000000000000000 ) ;
#175 = CARTESIAN_POINT ( 'NONE',  ( 0.000000000000000000, -9.374578970469563899, -10.68280860024325030 ) ) ;
#176 = DIRECTION ( 'NONE',  ( 1.000000000000000000, 0.000000000000000000, -0.000000000000000000 ) ) ;
#177 = AXIS2_PLACEMENT_3D ( 'NONE', #10882, #7123, #16164 ) ;
#178 = CIRCLE ( 'NONE', #11833, 18.49999999999999645 ) ;
#179 = DIRECTION ( 'NONE',  ( 0.000000000000000000, 0.000000000000000000, 1.000000000000000000 ) ) ;
#180 = ORIENTED_EDGE ( 'NONE', *, *, #12174, .T. ) ;
#181 = AXIS2_PLACEMENT_3D ( 'NONE', #13269, #18906, #9720 ) ;
#182 = ORIENTED_EDGE ( 'NONE', *, *, #11342, .T. ) ;
#183 = EDGE_CURVE ( 'NONE', #7231, #23927, #13888, .T. ) ;
#184 = DIRECTION ( 'NONE',  ( -0.000000000000000000, -0.000000000000000000, -1.000000000000000000 ) ) ;
#185 = EDGE_LOOP ( 'NONE', ( #17761, #2920, #15803, #19074 ) ) ;
#186 = EDGE_CURVE ( 'NONE', #13664, #23091, #13200, .T. ) ;
#187 = CARTESIAN_POINT ( 'NONE',  ( 39.50000000000000000, 15.50000000000000533, 19.70000000000000284 ) ) ;
#188 = CARTESIAN_POINT ( 'NONE',  ( 81.85249911436491743, -5.000000000000000000, 6.123233995736775157E-16 ) ) ;
#189 = LINE ( 'NONE', #16870, #10641 ) ;
#190 = AXIS2_PLACEMENT_3D ( 'NONE', #9359, #5489, #18425 ) ;
#191 = DIRECTION ( 'NONE',  ( -0.000000000000000000, -0.000000000000000000, -1.000000000000000000 ) ) ;
#192 = VERTEX_POINT ( 'NONE', #13627 ) ;
#193 = CARTESIAN_POINT ( 'NONE',  ( 0.000000000000000000, 0.000000000000000000, 12.50000000000000000 ) ) ;
#194 = DIRECTION ( 'NONE',  ( 0.000000000000000000, 0.000000000000000000, -1.000000000000000000 ) ) ;
#195 = ORIENTED_EDGE ( 'NONE', *, *, #4432, .F. ) ;
#196 = AXIS2_PLACEMENT_3D ( 'NONE', #4515, #15001, #11919 ) ;
#197 = ORIENTED_EDGE ( 'NONE', *, *, #13447, .T. ) ;
#198 = CARTESIAN_POINT ( 'NONE',  ( 6.809999908187194197E-13, -9.988891130263535700, 11.55958914175814201 ) ) ;
#199 = EDGE_LOOP ( 'NONE', ( #820, #16806, #2871, #170, #5990, #4363, #16078, #14680, #17872, #2627, #23157, #1528, #15276, #9674 ) ) ;
#200 = AXIS2_PLACEMENT_3D ( 'NONE', #19506, #8617, #6317 ) ;
#201 = PRODUCT_CONTEXT ( 'NONE', #6527, 'mechanical' ) ;
#202 = CIRCLE ( 'NONE', #22024, 5.099999999999996980 ) ;
#203 = ORIENTED_EDGE ( 'NONE', *, *, #19719, .T. ) ;
#204 = ORIENTED_EDGE ( 'NONE', *, *, #22334, .T. ) ;
#205 = DIRECTION ( 'NONE',  ( 1.360567432138674300E-16, -1.000000000000000000, 0.000000000000000000 ) ) ;
#206 = CARTESIAN_POINT ( 'NONE',  ( -2.682529543899159208, -8.255977015246598327, -12.03316557810918930 ) ) ;
#207 = CARTESIAN_POINT ( 'NONE',  ( 35.99999999999999289, -51.00000000000000711, 0.5000000000000000000 ) ) ;
#208 = VERTEX_POINT ( 'NONE', #21068 ) ;
#209 = CARTESIAN_POINT ( 'NONE',  ( 33.99999999999998579, -5.000000000000013323, 9.500000000000000000 ) ) ;
#210 = CARTESIAN_POINT ( 'NONE',  ( 71.67068093254673045, 7.562528597612068045E-15, 0.000000000000000000 ) ) ;
#211 = DIRECTION ( 'NONE',  ( 0.000000000000000000, 0.000000000000000000, 1.000000000000000000 ) ) ;
#212 = AXIS2_PLACEMENT_3D ( 'NONE', #21682, #3240, #1302 ) ;
#213 = DIRECTION ( 'NONE',  ( 1.000000000000000000, 0.000000000000000000, 0.000000000000000000 ) ) ;
#214 = DIRECTION ( 'NONE',  ( -0.000000000000000000, -0.000000000000000000, -1.000000000000000000 ) ) ;
#215 = AXIS2_PLACEMENT_3D ( 'NONE', #19096, #13347, #6619 ) ;
#216 = EDGE_CURVE ( 'NONE', #14151, #15740, #21331, .T. ) ;
#217 = ADVANCED_FACE ( 'NONE', ( #8123 ), #8920, .F. ) ;
#218 = ORIENTED_EDGE ( 'NONE', *, *, #1350, .T. ) ;
#219 = DIRECTION ( 'NONE',  ( 0.000000000000000000, -1.000000000000000000, 0.000000000000000000 ) ) ;
#220 = DIRECTION ( 'NONE',  ( -0.000000000000000000, -1.000000000000000000, -0.000000000000000000 ) ) ;
#221 = DIRECTION ( 'NONE',  ( -1.000000000000000000, -1.224606353822377258E-16, -0.000000000000000000 ) ) ;
#222 = CARTESIAN_POINT ( 'NONE',  ( 0.000000000000000000, -45.00000000000000000, 23.99999999999999645 ) ) ;
#223 = AXIS2_PLACEMENT_3D ( 'NONE', #2703, #9882, #642 ) ;
#224 = CONICAL_SURFACE ( 'NONE', #13854, 5.000000000000007994, 0.9599310885968855844 ) ;
#225 = CARTESIAN_POINT ( 'NONE',  ( -21.84999999999999787, 16.67999999999985405, 13.00000000000000178 ) ) ;
#226 = DIRECTION ( 'NONE',  ( 0.000000000000000000, 0.000000000000000000, 1.000000000000000000 ) ) ;
#227 = FILL_AREA_STYLE ('',( #11405 ) ) ;
#228 = ORIENTED_EDGE ( 'NONE', *, *, #4150, .T. ) ;
#229 = ORIENTED_EDGE ( 'NONE', *, *, #6879, .F. ) ;
#230 = VERTEX_POINT ( 'NONE', #4246 ) ;
#231 = ORIENTED_EDGE ( 'NONE', *, *, #12229, .F. ) ;
#232 = CIRCLE ( 'NONE', #1408, 5.000000000000007994 ) ;
#233 = CARTESIAN_POINT ( 'NONE',  ( 39.99999999999999289, 29.50000000000000000, 27.00000000000000000 ) ) ;
#234 = DIRECTION ( 'NONE',  ( 0.000000000000000000, 0.5406408174555987767, -0.8412535328311804284 ) ) ;
#235 = AXIS2_PLACEMENT_3D ( 'NONE', #20947, #21054, #11640 ) ;
#236 = EDGE_CURVE ( 'NONE', #7706, #21692, #11, .T. ) ;
#237 = CARTESIAN_POINT ( 'NONE',  ( -40.00000000000000000, 28.80990663662251450, 12.00000000000000000 ) ) ;
#238 = LINE ( 'NONE', #6083, #8802 ) ;
#239 = FILL_AREA_STYLE ('',( #18759 ) ) ;
#240 = CARTESIAN_POINT ( 'NONE',  ( -2.935661446562617183, 9.035036904803758873, -5.806742014460233747 ) ) ;
#241 = EDGE_CURVE ( 'NONE', #18499, #20393, #5403, .T. ) ;
#242 = DIRECTION ( 'NONE',  ( 1.000000000000000000, 0.000000000000000000, 0.000000000000000000 ) ) ;
#243 = EDGE_LOOP ( 'NONE', ( #6237, #14444, #13693, #2734 ) ) ;
#244 = B_SPLINE_CURVE_WITH_KNOTS ( 'NONE', 3,
 ( #16018, #23954, #6888, #18227 ),
 .UNSPECIFIED., .F., .F.,
 ( 4, 4 ),
 ( 0.000000000000000000, 0.8197781486845410193 ),
 .UNSPECIFIED. ) ;
#245 = ADVANCED_FACE ( 'NONE', ( #4620, #9951 ), #15830, .F. ) ;
#246 = CARTESIAN_POINT ( 'NONE',  ( -40.77574956473004164, -27.49633847812775755, 0.000000000000000000 ) ) ;
#247 = EDGE_CURVE ( 'NONE', #17382, #16656, #7759, .T. ) ;
#248 = AXIS2_PLACEMENT_3D ( 'NONE', #20687, #17137, #12870 ) ;
#249 = DIRECTION ( 'NONE',  ( 0.000000000000000000, 0.000000000000000000, -1.000000000000000000 ) ) ;
#250 = LINE ( 'NONE', #18547, #2878 ) ;
#251 = EDGE_CURVE ( 'NONE', #498, #18820, #12021, .T. ) ;
#252 = CARTESIAN_POINT ( 'NONE',  ( -17.15242344757784565, 8.297343789534778580, -4.632629386303500851 ) ) ;
#253 = AXIS2_PLACEMENT_3D ( 'NONE', #18403, #14486, #19889 ) ;
#254 = CARTESIAN_POINT ( 'NONE',  ( -31.74999999999995737, 6.123233995736767268E-16, -5.000000000000000888 ) ) ;
#255 = ORIENTED_EDGE ( 'NONE', *, *, #478, .T. ) ;
#256 = VECTOR ( 'NONE', #12691, 1000.000000000000000 ) ;
#257 = ORIENTED_EDGE ( 'NONE', *, *, #13116, .F. ) ;
#258 = PLANE ( 'NONE',  #10310 ) ;
#259 = ORIENTED_EDGE ( 'NONE', *, *, #11803, .F. ) ;
#260 = DIRECTION ( 'NONE',  ( 0.000000000000000000, -1.000000000000000000, 0.000000000000000000 ) ) ;
#261 = ORIENTED_EDGE ( 'NONE', *, *, #13949, .F. ) ;
#262 = CARTESIAN_POINT ( 'NONE',  ( 68.18181818181818699, 4.172000000000015696, 5.109226446042767468E-16 ) ) ;
#263 = CARTESIAN_POINT ( 'NONE',  ( 62.36363636363636687, 7.491529369508391930E-15, 0.000000000000000000 ) ) ;
#264 = DIRECTION ( 'NONE',  ( 0.000000000000000000, 0.000000000000000000, 1.000000000000000000 ) ) ;
#265 = DIRECTION ( 'NONE',  ( 1.000000000000000000, 0.000000000000000000, 0.000000000000000000 ) ) ;
#266 = AXIS2_PLACEMENT_3D ( 'NONE', #4476, #17261, #19473 ) ;
#267 = AXIS2_PLACEMENT_3D ( 'NONE', #15943, #21915, #14227 ) ;
#268 = EDGE_CURVE ( 'NONE', #16760, #20840, #2329, .T. ) ;
#269 = VECTOR ( 'NONE', #8708, 1000.000000000000000 ) ;
#270 = DIRECTION ( 'NONE',  ( 0.000000000000000000, 0.000000000000000000, 1.000000000000000000 ) ) ;
#271 = AXIS2_PLACEMENT_3D ( 'NONE', #14619, #3409, #18293 ) ;
#272 = CARTESIAN_POINT ( 'NONE',  ( 2.935661446561383503, 9.035036904804158553, -6.459589141758144137 ) ) ;
#273 = ORIENTED_EDGE ( 'NONE', *, *, #2065, .T. ) ;
#274 = CARTESIAN_POINT ( 'NONE',  ( -2.935661446562617183, 9.035036904803758873, 11.80674201446023375 ) ) ;
#275 = EDGE_CURVE ( 'NONE', #13326, #18344, #10190, .T. ) ;
#276 = ORIENTED_EDGE ( 'NONE', *, *, #7622, .T. ) ;
#277 = DIRECTION ( 'NONE',  ( -0.5735764363510517105, -0.8191520442889879128, 0.000000000000000000 ) ) ;
#278 = DIRECTION ( 'NONE',  ( -0.000000000000000000, -0.000000000000000000, 1.000000000000000000 ) ) ;
#279 = FACE_BOUND ( 'NONE', #20917, .T. ) ;
#280 = CARTESIAN_POINT ( 'NONE',  ( 41.00000000000000000, 5.999999999999986677, 12.00000000000000000 ) ) ;
#281 = CARTESIAN_POINT ( 'NONE',  ( 9.324366632326096311E-16, 9.000000000000000000, 77.99999999999998579 ) ) ;
#282 = VECTOR ( 'NONE', #12810, 1000.000000000000000 ) ;
#283 = CARTESIAN_POINT ( 'NONE',  ( 2.935661446561383503, 9.035036904804158553, -7.606742014460233570 ) ) ;
#284 = DIRECTION ( 'NONE',  ( -1.000000000000000000, -0.000000000000000000, 0.000000000000000000 ) ) ;
#285 = PRESENTATION_STYLE_ASSIGNMENT (( #11420 ) ) ;
#286 = CARTESIAN_POINT ( 'NONE',  ( -40.23082370883260239, 29.50000000000000711, -3.000000000000000000 ) ) ;
#287 = ORIENTED_EDGE ( 'NONE', *, *, #13188, .T. ) ;
#288 = LINE ( 'NONE', #12948, #17547 ) ;
#289 = CYLINDRICAL_SURFACE ( 'NONE', #1664, 17.87500000001787726 ) ;
#290 = CARTESIAN_POINT ( 'NONE',  ( 2.024999999999999911, 45.00000000000000000, -3.000000000000000000 ) ) ;
#291 = DIRECTION ( 'NONE',  ( 0.000000000000000000, 1.000000000000000000, 0.000000000000000000 ) ) ;
#292 = ORIENTED_EDGE ( 'NONE', *, *, #9808, .F. ) ;
#293 = ORIENTED_EDGE ( 'NONE', *, *, #1473, .F. ) ;
#294 = EDGE_CURVE ( 'NONE', #21978, #15166, #2770, .T. ) ;
#295 = ORIENTED_EDGE ( 'NONE', *, *, #2994, .F. ) ;
#296 = DIRECTION ( 'NONE',  ( 0.000000000000000000, -1.000000000000000000, 0.000000000000000000 ) ) ;
#297 = DIRECTION ( 'NONE',  ( -0.7071067811865469066, 8.659560562354941486E-17, -0.7071067811865482389 ) ) ;
#298 = ORIENTED_EDGE ( 'NONE', *, *, #19273, .F. ) ;
#299 = EDGE_CURVE ( 'NONE', #3391, #4737, #19089, .T. ) ;
#300 = CARTESIAN_POINT ( 'NONE',  ( 0.000000000000000000, -45.00000000000000000, 0.000000000000000000 ) ) ;
#301 = EDGE_LOOP ( 'NONE', ( #1823, #10414, #21595, #8457 ) ) ;
#302 = LINE ( 'NONE', #13461, #16288 ) ;
#303 = ORIENTED_EDGE ( 'NONE', *, *, #17244, .F. ) ;
#304 = DIRECTION ( 'NONE',  ( -1.000000000000000000, -1.224606353822377258E-16, -0.000000000000000000 ) ) ;
#305 = PLANE ( 'NONE',  #884 ) ;
#306 = DIRECTION ( 'NONE',  ( 1.000000000000000000, 0.000000000000000000, 0.000000000000000000 ) ) ;
#307 = DIRECTION ( 'NONE',  ( 0.000000000000000000, 1.000000000000000000, 0.000000000000000000 ) ) ;
#308 = ORIENTED_EDGE ( 'NONE', *, *, #9116, .T. ) ;
#309 = DIRECTION ( 'NONE',  ( -1.000000000000000000, -0.000000000000000000, 0.000000000000000000 ) ) ;
#310 = CARTESIAN_POINT ( 'NONE',  ( -31.74999999999995737, 0.000000000000000000, 5.000000000000000888 ) ) ;
#311 = CYLINDRICAL_SURFACE ( 'NONE', #7242, 5.099999999999996980 ) ;
#312 = ORIENTED_EDGE ( 'NONE', *, *, #2580, .F. ) ;
#313 = CIRCLE ( 'NONE', #1505, 1.000000000000000222 ) ;
#314 = EDGE_LOOP ( 'NONE', ( #13225, #21297, #22979, #6998 ) ) ;
#315 = CARTESIAN_POINT ( 'NONE',  ( 8.680847955711007202, 5.912916378492122225E-13, 4.633165578109188942 ) ) ;
#316 = ORIENTED_EDGE ( 'NONE', *, *, #1276, .T. ) ;
#317 = EDGE_CURVE ( 'NONE', #105, #19051, #18113, .T. ) ;
#318 = ORIENTED_EDGE ( 'NONE', *, *, #12802, .F. ) ;
#319 = EDGE_LOOP ( 'NONE', ( #19236, #16639, #16046, #6958, #1125 ) ) ;
#320 = EDGE_CURVE ( 'NONE', #7241, #1813, #6074, .T. ) ;
#321 = DIRECTION ( 'NONE',  ( 0.5735764363510427177, -0.8191520442889941300, 1.003171929053527705E-16 ) ) ;
#322 = CARTESIAN_POINT ( 'NONE',  ( 8.680847955711199049, -2.820578480813074496, -10.53316557810918752 ) ) ;
#323 = EDGE_LOOP ( 'NONE', ( #18331, #15250, #4632, #9150, #8336 ) ) ;
#324 = CARTESIAN_POINT ( 'NONE',  ( -40.00000000000000000, -29.49999999999999645, 11.00000000000000000 ) ) ;
#325 = CARTESIAN_POINT ( 'NONE',  ( -2.999999999999999112, 111.0000000000000000, 80.99999999999998579 ) ) ;
#326 = CARTESIAN_POINT ( 'NONE',  ( 29.00000000000000000, 29.50000000000000355, 12.00000000000000000 ) ) ;
#327 = CIRCLE ( 'NONE', #7697, 5.100000000000000533 ) ;
#328 = CARTESIAN_POINT ( 'NONE',  ( 20.84999999999999432, -15.04000000000000270, -25.00000000000000000 ) ) ;
#329 = FACE_OUTER_BOUND ( 'NONE', #7660, .T. ) ;
#330 = ORIENTED_EDGE ( 'NONE', *, *, #3431, .F. ) ;
#331 = CARTESIAN_POINT ( 'NONE',  ( 64.39795365981944997, 7.562528597612068045E-15, 0.000000000000000000 ) ) ;
#332 = DIRECTION ( 'NONE',  ( -0.000000000000000000, -0.000000000000000000, -1.000000000000000000 ) ) ;
#333 = DIRECTION ( 'NONE',  ( -0.7052211081716905916, 0.7089874389501501506, 0.000000000000000000 ) ) ;
#334 = CARTESIAN_POINT ( 'NONE',  ( 23.00000000000000000, -0.09016380984471503157, 11.68615217844040544 ) ) ;
#335 = DIRECTION ( 'NONE',  ( 1.000000000000000000, 0.000000000000000000, -0.000000000000000000 ) ) ;
#336 = DIRECTION ( 'NONE',  ( 1.000000000000000000, 0.000000000000000000, 0.000000000000000000 ) ) ;
#337 = DIRECTION ( 'NONE',  ( 1.000000000000000000, 0.000000000000000000, 0.000000000000000000 ) ) ;
#338 = EDGE_LOOP ( 'NONE', ( #9673, #2641, #5276, #22017 ) ) ;
#339 = EDGE_LOOP ( 'NONE', ( #15226, #6404, #14230 ) ) ;
#340 = CARTESIAN_POINT ( 'NONE',  ( -9.500000000000211386, 3.086737114211961064, 4.106742014460232681 ) ) ;
#341 = ORIENTED_EDGE ( 'NONE', *, *, #8197, .F. ) ;
#342 = CIRCLE ( 'NONE', #12784, 5.000000000000007994 ) ;
#343 = ADVANCED_FACE ( 'NONE', ( #587, #10447 ), #18147, .F. ) ;
#344 = LINE ( 'NONE', #20353, #1020 ) ;
#345 = UNCERTAINTY_MEASURE_WITH_UNIT (LENGTH_MEASURE( 1.000000000000000082E-05 ), #9120, 'distance_accuracy_value', 'NONE');
#346 = EDGE_CURVE ( 'NONE', #5306, #13831, #14026, .T. ) ;
#347 = CARTESIAN_POINT ( 'NONE',  ( 29.00000000000000355, 29.50000000000000000, 27.00000000000000000 ) ) ;
#348 = CARTESIAN_POINT ( 'NONE',  ( 0.000000000000000000, 15.03999999999999915, 25.00000000000000000 ) ) ;
#349 = CARTESIAN_POINT ( 'NONE',  ( 64.39795365981944997, 7.562528597612068045E-15, 0.000000000000000000 ) ) ;
#350 = CARTESIAN_POINT ( 'NONE',  ( 41.50000000000000000, -27.79189783386526358, 27.00000000000000000 ) ) ;
#351 = VECTOR ( 'NONE', #19301, 1000.000000000000000 ) ;
#352 = CARTESIAN_POINT ( 'NONE',  ( -23.85000000000000497, 15.03999999999999915, 25.00000000000000000 ) ) ;
#353 = EDGE_LOOP ( 'NONE', ( #15923, #14823, #11510, #16658 ) ) ;
#354 = DIRECTION ( 'NONE',  ( 0.000000000000000000, 0.000000000000000000, 1.000000000000000000 ) ) ;
#355 = LINE ( 'NONE', #16801, #10958 ) ;
#356 = FACE_OUTER_BOUND ( 'NONE', #319, .T. ) ;
#357 = CARTESIAN_POINT ( 'NONE',  ( -16.44572538483723534, 6.755397553796130161, -6.683320200552557822 ) ) ;
#358 = SHAPE_REPRESENTATION ( 'spur gear_am_Metric - Spur gear 2.75M 11T 20PA 23FW ---S11N75H50L18N', ( #8005 ), #18550 ) ;
#359 = FACE_OUTER_BOUND ( 'NONE', #2138, .T. ) ;
#360 = ORIENTED_EDGE ( 'NONE', *, *, #21024, .F. ) ;
#361 = CARTESIAN_POINT ( 'NONE',  ( -8.680847955711007202, -5.923547351154968927E-13, -7.633165578109188942 ) ) ;
#362 = PRODUCT_RELATED_PRODUCT_CATEGORY ( 'part', '', ( #43 ) ) ;
#363 = DIRECTION ( 'NONE',  ( 0.000000000000000000, 0.000000000000000000, -1.000000000000000000 ) ) ;
#364 = EDGE_LOOP ( 'NONE', ( #5051, #10753, #2893, #23678 ) ) ;
#365 = ADVANCED_FACE ( 'NONE', ( #20098 ), #2718, .T. ) ;
#366 = ORIENTED_EDGE ( 'NONE', *, *, #7622, .F. ) ;
#367 = DIRECTION ( 'NONE',  ( 0.000000000000000000, 0.000000000000000000, 1.000000000000000000 ) ) ;
#368 = ORIENTED_EDGE ( 'NONE', *, *, #10861, .T. ) ;
#369 = DIRECTION ( 'NONE',  ( 1.000000000000000000, 0.000000000000000000, -0.000000000000000000 ) ) ;
#370 = EDGE_CURVE ( 'NONE', #12252, #3007, #15970, .T. ) ;
#371 = CARTESIAN_POINT ( 'NONE',  ( 0.2999999999999999889, 1.227821507548370807E-15, -10.02592346138681023 ) ) ;
#372 = DIRECTION ( 'NONE',  ( -0.000000000000000000, -0.000000000000000000, -1.000000000000000000 ) ) ;
#373 = EDGE_CURVE ( 'NONE', #12918, #20567, #14228, .T. ) ;
#374 = DIRECTION ( 'NONE',  ( -1.000000000000000000, -1.224606353822377258E-16, -0.000000000000000000 ) ) ;
#375 = ADVANCED_FACE ( 'NONE', ( #21572 ), #4239, .T. ) ;
#376 = CARTESIAN_POINT ( 'NONE',  ( 14.98952570844870102, -0.6468970097546504761, -9.483487670324114660 ) ) ;
#377 = CARTESIAN_POINT ( 'NONE',  ( -6.153822176767817416E-13, 9.500000000000000000, -3.500000000000014211 ) ) ;
#378 = FACE_BOUND ( 'NONE', #14789, .T. ) ;
#379 = VERTEX_POINT ( 'NONE', #12752 ) ;
#380 = CARTESIAN_POINT ( 'NONE',  ( 31.10231664966676846, 45.36128193761570770, 12.00000000000000000 ) ) ;
#381 = ORIENTED_EDGE ( 'NONE', *, *, #16023, .T. ) ;
#382 = CARTESIAN_POINT ( 'NONE',  ( -31.10231664966676135, -45.36128193761570770, -27.00000000000000000 ) ) ;
#383 = CONICAL_SURFACE ( 'NONE', #8934, 9.000000000000000000, 0.7853981633974473908 ) ;
#384 = DIRECTION ( 'NONE',  ( -1.000000000000000000, -1.224606353822377258E-16, -0.000000000000000000 ) ) ;
#385 = DIRECTION ( 'NONE',  ( -1.000000000000000000, 0.000000000000000000, 0.000000000000000000 ) ) ;
#386 = AXIS2_PLACEMENT_3D ( 'NONE', #7011, #19846, #23975 ) ;
#387 = LINE ( 'NONE', #4295, #12065 ) ;
#388 = CARTESIAN_POINT ( 'NONE',  ( -2.979928582684572724, 8.492451671845357097, 80.60107722653498286 ) ) ;
#389 = LINE ( 'NONE', #19303, #6735 ) ;
#390 = CARTESIAN_POINT ( 'NONE',  ( 0.000000000000000000, -14.99147757894464306, 7.750000000000000000 ) ) ;
#391 = EDGE_CURVE ( 'NONE', #5706, #4329, #3496, .T. ) ;
#392 = DIRECTION ( 'NONE',  ( -1.000000000000000000, 0.000000000000000000, 0.000000000000000000 ) ) ;
#393 = ORIENTED_EDGE ( 'NONE', *, *, #6106, .F. ) ;
#394 = CYLINDRICAL_SURFACE ( 'NONE', #10525, 9.500000000000000000 ) ;
#395 = CARTESIAN_POINT ( 'NONE',  ( 2.682529543899157876, 8.255977015246598327, 11.03316557810918752 ) ) ;
#396 = FACE_OUTER_BOUND ( 'NONE', #16377, .T. ) ;
#397 = CYLINDRICAL_SURFACE ( 'NONE', #14885, 1.499999999999998002 ) ;
#398 = EDGE_CURVE ( 'NONE', #9329, #12017, #10900, .T. ) ;
#399 = EDGE_CURVE ( 'NONE', #3497, #3956, #12631, .T. ) ;
#400 = ORIENTED_EDGE ( 'NONE', *, *, #1743, .F. ) ;
#402 = ORIENTED_EDGE ( 'NONE', *, *, #23393, .T. ) ;
#401 = AXIS2_PLACEMENT_3D ( 'NONE', #14857, #5613, #1490 ) ;
#403 = ITEM_DEFINED_TRANSFORMATION ( 'NONE', 'NONE', #6506,  #17768 ) ;
#404 = ORIENTED_EDGE ( 'NONE', *, *, #16817, .F. ) ;
#405 = DIRECTION ( 'NONE',  ( 0.000000000000000000, 1.000000000000000000, 0.000000000000000000 ) ) ;
#406 = CARTESIAN_POINT ( 'NONE',  ( 2.935661446562616295, -9.035036904803758873, -12.80674201446023375 ) ) ;
#407 = EDGE_LOOP ( 'NONE', ( #9562, #5623, #18724, #2423 ) ) ;
#408 = ORIENTED_EDGE ( 'NONE', *, *, #12855, .T. ) ;
#409 = DIRECTION ( 'NONE',  ( -1.000000000000000000, -0.000000000000000000, -0.000000000000000000 ) ) ;
#410 = DIRECTION ( 'NONE',  ( -0.000000000000000000, -0.000000000000000000, -1.000000000000000000 ) ) ;
#411 = VERTEX_POINT ( 'NONE', #10552 ) ;
#412 = CARTESIAN_POINT ( 'NONE',  ( -7.648716207067147721, -5.640964897112045406, -3.500655991556068880 ) ) ;
#413 = EDGE_LOOP ( 'NONE', ( #450, #8940, #2747, #24030 ) ) ;
#414 = DIRECTION ( 'NONE',  ( -1.000000000000000000, -0.000000000000000000, -0.000000000000000000 ) ) ;
#415 = DIRECTION ( 'NONE',  ( -1.000000000000000000, 0.000000000000000000, 0.000000000000000000 ) ) ;
#416 = DIRECTION ( 'NONE',  ( 1.000000000000000000, 0.000000000000000000, 0.000000000000000000 ) ) ;
#417 = FACE_BOUND ( 'NONE', #11319, .T. ) ;
#418 = AXIS2_PLACEMENT_3D ( 'NONE', #13567, #8055, #21010 ) ;
#419 = EDGE_LOOP ( 'NONE', ( #22193, #22078, #19514, #14610, #19694, #15843, #2106, #5083, #6149, #13689 ) ) ;
#420 = FACE_OUTER_BOUND ( 'NONE', #7295, .T. ) ;
#421 = DIRECTION ( 'NONE',  ( 0.000000000000000000, 1.000000000000000000, -1.295896757998780388E-15 ) ) ;
#422 = CARTESIAN_POINT ( 'NONE',  ( 23.00000000000000000, 11.90821470209334798, -7.758837095328730449 ) ) ;
#423 = ORIENTED_EDGE ( 'NONE', *, *, #9003, .F. ) ;
#424 = ORIENTED_EDGE ( 'NONE', *, *, #17118, .T. ) ;
#425 = CARTESIAN_POINT ( 'NONE',  ( 5.365059087799946447, -7.384370330706356178, 6.333165578109187344 ) ) ;
#426 = ORIENTED_EDGE ( 'NONE', *, *, #18283, .T. ) ;
#427 = ADVANCED_FACE ( 'NONE', ( #9089 ), #383, .T. ) ;
#428 = CARTESIAN_POINT ( 'NONE',  ( 23.00000000000000000, -8.772759796005177080, -7.720943453482119523 ) ) ;
#429 = ORIENTED_EDGE ( 'NONE', *, *, #19468, .F. ) ;
#430 = VERTEX_POINT ( 'NONE', #6920 ) ;
#431 = CARTESIAN_POINT ( 'NONE',  ( 80.39795365981946418, -5.000000000000000000, 6.123233995736775157E-16 ) ) ;
#432 = CARTESIAN_POINT ( 'NONE',  ( 0.000000000000000000, 0.000000000000000000, 0.000000000000000000 ) ) ;
#433 = DIRECTION ( 'NONE',  ( -1.000000000000000000, -1.224606353822377258E-16, -0.000000000000000000 ) ) ;
#434 = AXIS2_PLACEMENT_3D ( 'NONE', #1812, #20123, #9338 ) ;
#435 = ORIENTED_EDGE ( 'NONE', *, *, #2128, .F. ) ;
#436 = DIRECTION ( 'NONE',  ( 1.000000000000000000, 1.224606353822377258E-16, 0.000000000000000000 ) ) ;
#437 = DIRECTION ( 'NONE',  ( 0.000000000000000000, -1.000000000000000000, 0.000000000000000000 ) ) ;
#438 = DIRECTION ( 'NONE',  ( -1.000000000000000000, -1.224606353822377258E-16, -0.000000000000000000 ) ) ;
#439 = CARTESIAN_POINT ( 'NONE',  ( 0.000000000000000000, 0.000000000000000000, 0.000000000000000000 ) ) ;
#440 = AXIS2_PLACEMENT_3D ( 'NONE', #7629, #21934, #9229 ) ;
#441 = ORIENTED_EDGE ( 'NONE', *, *, #3295, .T. ) ;
#442 = CARTESIAN_POINT ( 'NONE',  ( 0.000000000000000000, 45.00000000000000000, -23.99999999999999645 ) ) ;
#443 = EDGE_CURVE ( 'NONE', #14074, #21725, #10459, .T. ) ;
#444 = ORIENTED_EDGE ( 'NONE', *, *, #13659, .T. ) ;
#445 = FILL_AREA_STYLE_COLOUR ( '', #5123 ) ;
#446 = DIRECTION ( 'NONE',  ( -0.000000000000000000, -0.000000000000000000, -1.000000000000000000 ) ) ;
#447 = DIRECTION ( 'NONE',  ( 0.000000000000000000, 0.000000000000000000, 1.000000000000000000 ) ) ;
#448 = EDGE_CURVE ( 'NONE', #4329, #14984, #23519, .T. ) ;
#449 = CARTESIAN_POINT ( 'NONE',  ( -41.99999999999999289, 0.000000000000000000, 10.50249999999999950 ) ) ;
#450 = ORIENTED_EDGE ( 'NONE', *, *, #7005, .F. ) ;
#451 = ORIENTED_EDGE ( 'NONE', *, *, #2942, .T. ) ;
#452 = AXIS2_PLACEMENT_3D ( 'NONE', #7409, #18546, #12906 ) ;
#453 = APPLICATION_CONTEXT ( 'automotive_design' ) ;
#454 = ADVANCED_FACE ( 'NONE', ( #19970, #10794 ), #8856, .T. ) ;
#455 = CONICAL_SURFACE ( 'NONE', #13345, 10.50249999999999950, 0.7853981633974491672 ) ;
#456 = CONICAL_SURFACE ( 'NONE', #16803, 5.000000000000007994, 0.9599310885968855844 ) ;
#457 = ORIENTED_EDGE ( 'NONE', *, *, #5013, .F. ) ;
#458 = DIRECTION ( 'NONE',  ( 0.000000000000000000, 0.000000000000000000, -1.000000000000000000 ) ) ;
#459 = CARTESIAN_POINT ( 'NONE',  ( -39.99999999999999289, 27.79189783386526358, -27.00000000000000000 ) ) ;
#460 = DIRECTION ( 'NONE',  ( 1.000000000000000000, 0.000000000000000000, 0.000000000000000000 ) ) ;
#461 = DIRECTION ( 'NONE',  ( -1.000000000000000000, -2.600433232233976523E-16, 0.000000000000000000 ) ) ;
#462 = LINE ( 'NONE', #2294, #13049 ) ;
#463 = DIRECTION ( 'NONE',  ( -0.000000000000000000, -0.000000000000000000, -1.000000000000000000 ) ) ;
#464 = ORIENTED_EDGE ( 'NONE', *, *, #22760, .F. ) ;
#465 = EDGE_LOOP ( 'NONE', ( #9953, #21029, #23711, #6044 ) ) ;
#466 = CARTESIAN_POINT ( 'NONE',  ( 29.99999999999998934, -1.387778780781445676E-14, 9.500000000000000000 ) ) ;
#467 = CIRCLE ( 'NONE', #14850, 4.172000000000008590 ) ;
#468 = CIRCLE ( 'NONE', #10586, 17.87500000001787726 ) ;
#469 = CIRCLE ( 'NONE', #3578, 5.999999999999998224 ) ;
#470 = DIRECTION ( 'NONE',  ( -0.000000000000000000, 0.000000000000000000, 1.000000000000000000 ) ) ;
#471 = DIRECTION ( 'NONE',  ( -1.000000000000000000, -0.000000000000000000, -0.000000000000000000 ) ) ;
#472 = LINE ( 'NONE', #7889, #101 ) ;
#473 = CONICAL_SURFACE ( 'NONE', #21125, 1.000000000000000222, 0.7853981633974508325 ) ;
#474 = CARTESIAN_POINT ( 'NONE',  ( 23.85000000000000142, -15.03999999999999737, 2.200000000000000178 ) ) ;
#475 = DIRECTION ( 'NONE',  ( 0.000000000000000000, 0.000000000000000000, 1.000000000000000000 ) ) ;
#476 = EDGE_CURVE ( 'NONE', #5201, #9670, #7337, .T. ) ;
#477 = ORIENTED_EDGE ( 'NONE', *, *, #22323, .F. ) ;
#478 = EDGE_CURVE ( 'NONE', #4642, #16254, #18018, .T. ) ;
#479 = CARTESIAN_POINT ( 'NONE',  ( -7.022953521755574080, 5.102474405759713783, -7.433165578109188765 ) ) ;
#480 = CYLINDRICAL_SURFACE ( 'NONE', #7582, 9.000000000000000000 ) ;
#481 = ORIENTED_EDGE ( 'NONE', *, *, #11661, .F. ) ;
#482 = ORIENTED_EDGE ( 'NONE', *, *, #4334, .T. ) ;
#483 = DIRECTION ( 'NONE',  ( -1.000000000000000000, -0.000000000000000000, -0.000000000000000000 ) ) ;
#484 = EDGE_LOOP ( 'NONE', ( #7271, #13067, #20079, #19929 ) ) ;
#485 = CARTESIAN_POINT ( 'NONE',  ( 0.000000000000000000, 4.685197434473818312, -1.301042606982605321E-15 ) ) ;
#486 = CIRCLE ( 'NONE', #7856, 8.000000000000003553 ) ;
#487 = VECTOR ( 'NONE', #22669, 1000.000000000000000 ) ;
#488 = AXIS2_PLACEMENT_3D ( 'NONE', #7572, #19067, #22602 ) ;
#489 = AXIS2_PLACEMENT_3D ( 'NONE', #4999, #8870, #14016 ) ;
#490 = DIRECTION ( 'NONE',  ( 0.000000000000000000, 0.000000000000000000, 1.000000000000000000 ) ) ;
#491 = VECTOR ( 'NONE', #23328, 1000.000000000000000 ) ;
#492 = CIRCLE ( 'NONE', #10208, 1.000000000000001998 ) ;
#493 = CIRCLE ( 'NONE', #13726, 11.00000000000001066 ) ;
#494 = LINE ( 'NONE', #20879, #9455 ) ;
#495 = CARTESIAN_POINT ( 'NONE',  ( 6.250000000000000000, -10.82531754730548279, 2.500000000000000000 ) ) ;
#496 =( BOUNDED_CURVE ( )  B_SPLINE_CURVE ( 2, ( #21372, #6721, #21614, #6228, #11953, #10242, #19421, #13671, #4911, #750, #2697 ),
 .UNSPECIFIED., .F., .T. ) 
 B_SPLINE_CURVE_WITH_KNOTS ( ( 3, 2, 2, 2, 2, 3 ),
 ( 0.006042316813507608332, 0.01999999999999999001, 0.03999999999999997308, 0.05999999999999994921, 0.07999999999999993228, 0.09999999999999992228 ),
 .UNSPECIFIED. ) 
 CURVE ( )  GEOMETRIC_REPRESENTATION_ITEM ( )  RATIONAL_B_SPLINE_CURVE ( ( 0.9793613297716612376, 0.9658431180202251554, 1.000000000000000000, 0.9510565162951535312, 1.000000000000000000, 0.9510565162951535312, 1.000000000000000000, 0.9510565162951535312, 1.000000000000000000, 0.9510565162951537532, 0.9999999999999997780 ) ) 
 REPRESENTATION_ITEM ( '' )  );
#497 = CARTESIAN_POINT ( 'NONE',  ( -2.935661446561384391, -9.035036904804158553, -3.459589141758144137 ) ) ;
#498 = VERTEX_POINT ( 'NONE', #8959 ) ;
#499 = EDGE_LOOP ( 'NONE', ( #19745, #2721, #11674, #16253 ) ) ;
#500 = DIRECTION ( 'NONE',  ( 0.000000000000000000, 1.000000000000000000, 0.000000000000000000 ) ) ;
#501 = DIRECTION ( 'NONE',  ( -1.000000000000000000, 0.000000000000000000, 0.000000000000000000 ) ) ;
#502 = CARTESIAN_POINT ( 'NONE',  ( 87.67068093254673045, 7.562528597612068045E-15, 0.000000000000000000 ) ) ;
#503 = ADVANCED_FACE ( 'NONE', ( #16404 ), #10677, .T. ) ;
#504 = VECTOR ( 'NONE', #5212, 1000.000000000000114 ) ;
#505 = DIRECTION ( 'NONE',  ( -0.000000000000000000, -0.000000000000000000, -1.000000000000000000 ) ) ;
#506 = ADVANCED_FACE ( 'NONE', ( #7023 ), #12862, .T. ) ;
#507 = CARTESIAN_POINT ( 'NONE',  ( -7.561939491010498671, 5.750397476200742375, -11.99999999999999822 ) ) ;
#508 = ADVANCED_FACE ( 'NONE', ( #14708 ), #11023, .T. ) ;
#509 = CARTESIAN_POINT ( 'NONE',  ( -9.500000000000000000, -6.482511860946779655E-13, -8.206742014460234103 ) ) ;
#510 = CIRCLE ( 'NONE', #21501, 17.87500000001787726 ) ;
#511 = AXIS2_PLACEMENT_3D ( 'NONE', #14794, #18599, #11234 ) ;
#512 = CARTESIAN_POINT ( 'NONE',  ( -9.500000000000000000, -6.482511860946779655E-13, 4.206742014460233214 ) ) ;
#513 = CARTESIAN_POINT ( 'NONE',  ( 7.685661446561619314, 5.583959896779020049, -5.406742014460233392 ) ) ;
#514 = EDGE_LOOP ( 'NONE', ( #9069, #10444 ) ) ;
#515 = AXIS2_PLACEMENT_3D ( 'NONE', #20081, #16040, #23502 ) ;
#516 = CARTESIAN_POINT ( 'NONE',  ( -40.89823313241237912, -26.41789760203349502, 27.00000000000000000 ) ) ;
#517 = CARTESIAN_POINT ( 'NONE',  ( -8.680847955711007202, -5.923547351154968927E-13, 7.633165578109188942 ) ) ;
#518 = AXIS2_PLACEMENT_3D ( 'NONE', #12701, #20041, #20167 ) ;
#519 = DIRECTION ( 'NONE',  ( 0.7089874389501492624, 0.7052211081716913688, 0.000000000000000000 ) ) ;
#520 = DIRECTION ( 'NONE',  ( 0.000000000000000000, -1.000000000000000000, 0.000000000000000000 ) ) ;
#521 = ORIENTED_EDGE ( 'NONE', *, *, #12887, .F. ) ;
#522 = ITEM_DEFINED_TRANSFORMATION ( 'NONE', 'NONE', #11496,  #8005 ) ;
#524 = AXIS2_PLACEMENT_3D ( 'NONE', #23308, #13770, #15848 ) ;
#523 = LINE ( 'NONE', #2717, #14616 ) ;
#525 = AXIS2_PLACEMENT_3D ( 'NONE', #6258, #4452, #15781 ) ;
#526 = CIRCLE ( 'NONE', #18452, 18.49999999999999645 ) ;
#527 = ADVANCED_FACE ( 'NONE', ( #7269 ), #16537, .T. ) ;
#528 = CARTESIAN_POINT ( 'NONE',  ( 2.935661446561383503, 9.035036904804158553, -9.606742014460232681 ) ) ;
#529 = ORIENTED_EDGE ( 'NONE', *, *, #1014, .F. ) ;
#530 = VERTEX_POINT ( 'NONE', #17315 ) ;
#531 = AXIS2_PLACEMENT_3D ( 'NONE', #1963, #11466, #5767 ) ;
#532 = AXIS2_PLACEMENT_3D ( 'NONE', #21236, #9733, #4537 ) ;
#533 = ORIENTED_EDGE ( 'NONE', *, *, #9981, .T. ) ;
#534 = CARTESIAN_POINT ( 'NONE',  ( -3.064960521623495637, -8.996099670591407360, -3.501175347612584421 ) ) ;
#535 = EDGE_CURVE ( 'NONE', #12646, #12980, #16343, .T. ) ;
#536 = ORIENTED_EDGE ( 'NONE', *, *, #3636, .F. ) ;
#537 = ADVANCED_FACE ( 'NONE', ( #2678 ), #12172, .T. ) ;
#538 = DIRECTION ( 'NONE',  ( -0.000000000000000000, -0.000000000000000000, -1.000000000000000000 ) ) ;
#539 = CARTESIAN_POINT ( 'NONE',  ( -17.25000000000000000, 15.50000000000000000, 14.70000000000000284 ) ) ;
#540 = LINE ( 'NONE', #22618, #14924 ) ;
#541 = CARTESIAN_POINT ( 'NONE',  ( 29.00000000000000355, -29.50000000000000000, -3.000000000000000000 ) ) ;
#542 = ORIENTED_EDGE ( 'NONE', *, *, #18708, .T. ) ;
#543 = CYLINDRICAL_SURFACE ( 'NONE', #962, 5.000000000000000888 ) ;
#544 = DIRECTION ( 'NONE',  ( -0.000000000000000000, -0.000000000000000000, 1.000000000000000000 ) ) ;
#545 = ORIENTED_EDGE ( 'NONE', *, *, #20956, .F. ) ;
#546 = CONICAL_SURFACE ( 'NONE', #6785, 5.000000000000007994, 0.9599310885968855844 ) ;
#547 = EDGE_LOOP ( 'NONE', ( #14292, #13702, #6261, #2259 ) ) ;
#548 = CARTESIAN_POINT ( 'NONE',  ( 2.682529543900284974, -8.255977015246234174, 6.233165578109188587 ) ) ;
#549 = ORIENTED_EDGE ( 'NONE', *, *, #21450, .T. ) ;
#550 = AXIS2_PLACEMENT_3D ( 'NONE', #11975, #19444, #2723 ) ;
#551 = ORIENTED_EDGE ( 'NONE', *, *, #872, .T. ) ;
#552 = VECTOR ( 'NONE', #2265, 1000.000000000000114 ) ;
#553 = CARTESIAN_POINT ( 'NONE',  ( -2.935661446561384391, -9.035036904804158553, 5.459589141758144137 ) ) ;
#554 = CIRCLE ( 'NONE', #181, 1.499999999999999556 ) ;
#555 = VERTEX_POINT ( 'NONE', #21228 ) ;
#556 = VERTEX_POINT ( 'NONE', #8143 ) ;
#557 = FACE_OUTER_BOUND ( 'NONE', #10768, .T. ) ;
#558 = CARTESIAN_POINT ( 'NONE',  ( -8.680847955711200825, 2.820578480813073607, -3.533165578109187965 ) ) ;
#559 = LINE ( 'NONE', #6165, #2084 ) ;
#560 = ADVANCED_FACE ( 'NONE', ( #19147 ), #6469, .F. ) ;
#561 = ORIENTED_EDGE ( 'NONE', *, *, #17545, .F. ) ;
#562 = DIRECTION ( 'NONE',  ( 0.000000000000000000, 0.000000000000000000, 1.000000000000000000 ) ) ;
#563 = LINE ( 'NONE', #19228, #13900 ) ;
#564 = CARTESIAN_POINT ( 'NONE',  ( 0.000000000000000000, -45.00000000000000000, -8.673617379884035472E-16 ) ) ;
#565 = FACE_OUTER_BOUND ( 'NONE', #11351, .T. ) ;
#566 = VERTEX_POINT ( 'NONE', #6593 ) ;
#567 = CARTESIAN_POINT ( 'NONE',  ( 0.000000000000000000, -13.61176534793449200, 4.089617900950054619 ) ) ;
#568 = PRESENTATION_LAYER_ASSIGNMENT (  '', '', ( #12636 ) ) ;
#569 = VERTEX_POINT ( 'NONE', #6215 ) ;
#570 = CARTESIAN_POINT ( 'NONE',  ( -1.029124893018731811E-15, -45.00000000000000000, -22.79827876194487857 ) ) ;
#571 = ADVANCED_FACE ( 'NONE', ( #2427 ), #17549, .T. ) ;
#572 = DIRECTION ( 'NONE',  ( 0.000000000000000000, -1.000000000000000000, 0.000000000000000000 ) ) ;
#573 = AXIS2_PLACEMENT_3D ( 'NONE', #9273, #14531, #16720 ) ;
#574 = CARTESIAN_POINT ( 'NONE',  ( -41.73082370883260239, 27.62204025492845361, -3.000000000000000000 ) ) ;
#575 = AXIS2_PLACEMENT_3D ( 'NONE', #18030, #1330, #15708 ) ;
#576 = CYLINDRICAL_SURFACE ( 'NONE', #22798, 6.050000000006051870 ) ;
#577 = CARTESIAN_POINT ( 'NONE',  ( 2.682529543900284974, -8.255977015246234174, -8.233165578109190363 ) ) ;
#578 = VERTEX_POINT ( 'NONE', #22821 ) ;
#579 = SURFACE_SIDE_STYLE ('',( #22786 ) ) ;
#580 = ORIENTED_EDGE ( 'NONE', *, *, #22981, .F. ) ;
#581 = VERTEX_POINT ( 'NONE', #8030 ) ;
#582 = CARTESIAN_POINT ( 'NONE',  ( -7.022953521755574080, 5.102474405759713783, 9.433165578109189653 ) ) ;
#583 = ORIENTED_EDGE ( 'NONE', *, *, #20637, .F. ) ;
#584 = CARTESIAN_POINT ( 'NONE',  ( 693.7818939062880190, 888.4837211537981148, 1347.481724745927977 ) ) ;
#585 = AXIS2_PLACEMENT_3D ( 'NONE', #2571, #21363, #17444 ) ;
#586 = VECTOR ( 'NONE', #1373, 1000.000000000000114 ) ;
#587 = FACE_BOUND ( 'NONE', #13497, .T. ) ;
#588 = VERTEX_POINT ( 'NONE', #4531 ) ;
#589 = CARTESIAN_POINT ( 'NONE',  ( 5.871322893123449127, 8.081182679344781405, -10.35958914175814627 ) ) ;
#590 = PRODUCT_DEFINITION_CONTEXT ( 'detailed design', #14437, 'design' ) ;
#591 = EDGE_CURVE ( 'NONE', #20973, #8446, #20260, .T. ) ;
#592 = CIRCLE ( 'NONE', #11071, 17.87500000001787726 ) ;
#593 = CIRCLE ( 'NONE', #14217, 11.00000000000000711 ) ;
#594 = CARTESIAN_POINT ( 'NONE',  ( 7.121611749575534667, -5.132745777193459702, 12.50000000000000533 ) ) ;
#595 = CARTESIAN_POINT ( 'NONE',  ( 2.879195777975148768E-17, 1.227821507548370807E-15, -10.02592346138681023 ) ) ;
#596 = CARTESIAN_POINT ( 'NONE',  ( 10.40000000000000036, 0.000000000000000000, 0.000000000000000000 ) ) ;
#597 = ADVANCED_FACE ( 'NONE', ( #13913 ), #1452, .F. ) ;
#598 = VERTEX_POINT ( 'NONE', #10983 ) ;
#599 = LINE ( 'NONE', #9963, #8749 ) ;
#600 = AXIS2_PLACEMENT_3D ( 'NONE', #18888, #17417, #17043 ) ;
#601=STYLED_ITEM('',(#24155),#2929);
#602 = CARTESIAN_POINT ( 'NONE',  ( 76.32931906745326955, -4.999999999999989342, 0.000000000000000000 ) ) ;
#603 = ADVANCED_FACE ( 'NONE', ( #24066 ), #23395, .F. ) ;
#604 = LINE ( 'NONE', #20609, #11879 ) ;
#605 = CARTESIAN_POINT ( 'NONE',  ( -6.249999999999999112, -10.82531754730548279, 2.500000000000000000 ) ) ;
#606 = EDGE_CURVE ( 'NONE', #18123, #12662, #6674, .T. ) ;
#607 = CARTESIAN_POINT ( 'NONE',  ( 18.50000000000000000, 2.265596578422603396E-15, 15.50000000000000000 ) ) ;
#608 = CARTESIAN_POINT ( 'NONE',  ( -18.50000000000000000, 0.000000000000000000, 0.000000000000000000 ) ) ;
#609 = CARTESIAN_POINT ( 'NONE',  ( -9.500000000000000000, -6.482511860946779655E-13, 4.206742014460233214 ) ) ;
#610 = CARTESIAN_POINT ( 'NONE',  ( 5.365059087799946447, -7.384370330706356178, -6.333165578109187344 ) ) ;
#611 = ORIENTED_EDGE ( 'NONE', *, *, #3056, .F. ) ;
#612 = ORIENTED_EDGE ( 'NONE', *, *, #16152, .T. ) ;
#613 = FACE_OUTER_BOUND ( 'NONE', #4176, .T. ) ;
#614 = DIRECTION ( 'NONE',  ( 0.000000000000000000, -0.000000000000000000, 1.000000000000000000 ) ) ;
#615 = AXIS2_PLACEMENT_3D ( 'NONE', #6424, #7742, #9691 ) ;
#616 = ORIENTED_EDGE ( 'NONE', *, *, #19811, .F. ) ;
#617 = AXIS2_PLACEMENT_3D ( 'NONE', #4422, #21255, #2953 ) ;
#618 = CARTESIAN_POINT ( 'NONE',  ( 21.13207267780287069, -38.32709852940855910, 12.00000000000000000 ) ) ;
#619 = DIRECTION ( 'NONE',  ( 0.000000000000000000, 0.000000000000000000, 1.000000000000000000 ) ) ;
#620 = ORIENTED_EDGE ( 'NONE', *, *, #1134, .T. ) ;
#621 = DIRECTION ( 'NONE',  ( -0.000000000000000000, -0.000000000000000000, -1.000000000000000000 ) ) ;
#622 = EDGE_CURVE ( 'NONE', #5826, #19489, #1182, .T. ) ;
#623 = DIRECTION ( 'NONE',  ( 1.000000000000000000, 0.000000000000000000, 0.000000000000000000 ) ) ;
#624 = DIRECTION ( 'NONE',  ( -0.7071067811865660024, 8.659560562355159656E-17, 0.7071067811865291430 ) ) ;
#625 = LINE ( 'NONE', #9500, #16822 ) ;
#626 = EDGE_CURVE ( 'NONE', #16958, #12954, #12793, .T. ) ;
#627 = AXIS2_PLACEMENT_3D ( 'NONE', #21072, #23298, #6451 ) ;
#628 = AXIS2_PLACEMENT_3D ( 'NONE', #8146, #17682, #17438 ) ;
#630 = EDGE_CURVE ( 'NONE', #7385, #14193, #9403, .T. ) ;
#629 = DIRECTION ( 'NONE',  ( -1.000000000000000000, -1.224606353822377258E-16, -0.000000000000000000 ) ) ;
#631 = ORIENTED_EDGE ( 'NONE', *, *, #5431, .T. ) ;
#632 = FACE_OUTER_BOUND ( 'NONE', #10818, .T. ) ;
#633 = CIRCLE ( 'NONE', #6869, 49.99999999999998579 ) ;
#634 = ORIENTED_EDGE ( 'NONE', *, *, #9707, .T. ) ;
#635 = CARTESIAN_POINT ( 'NONE',  ( -10.00000000000000000, 0.000000000000000000, 0.000000000000000000 ) ) ;
#636 = CARTESIAN_POINT ( 'NONE',  ( 0.000000000000000000, 15.23000000000000220, -27.00000000000000000 ) ) ;
#637 =( NAMED_UNIT ( * ) SI_UNIT ( $, .STERADIAN. ) SOLID_ANGLE_UNIT ( ) );
#638 = CIRCLE ( 'NONE', #11898, 2.000000000000000000 ) ;
#639 = CARTESIAN_POINT ( 'NONE',  ( -39.00000000000000000, 0.000000000000000000, 11.00000000000000000 ) ) ;
#640 = CARTESIAN_POINT ( 'NONE',  ( -0.7829208760733560313, 8.967963617333239768, 78.09729311758064796 ) ) ;
#641 = CYLINDRICAL_SURFACE ( 'NONE', #21938, 11.68650000001168721 ) ;
#642 = DIRECTION ( 'NONE',  ( 0.000000000000000000, -1.000000000000000000, 0.000000000000000000 ) ) ;
#643 = ORIENTED_EDGE ( 'NONE', *, *, #13151, .T. ) ;
#644 = CARTESIAN_POINT ( 'NONE',  ( -6.822232771736903637E-13, 9.988891130263535700, -7.706742014460232326 ) ) ;
#645 = ORIENTED_EDGE ( 'NONE', *, *, #164, .F. ) ;
#646 = DIRECTION ( 'NONE',  ( -1.000000000000000000, 0.000000000000000000, -0.000000000000000000 ) ) ;
#647 = CARTESIAN_POINT ( 'NONE',  ( 7.022953521754877748, 5.102474405760673903, 6.833165578109188232 ) ) ;
#648 = DIRECTION ( 'NONE',  ( -1.000000000000000000, 0.000000000000000000, 0.000000000000000000 ) ) ;
#649 = AXIS2_PLACEMENT_3D ( 'NONE', #23008, #23137, #15541 ) ;
#650 = CARTESIAN_POINT ( 'NONE',  ( 67.30704456891035647, 7.562528597612068045E-15, 0.000000000000000000 ) ) ;
#651 =( GEOMETRIC_REPRESENTATION_CONTEXT ( 3 ) GLOBAL_UNCERTAINTY_ASSIGNED_CONTEXT ( ( #2290 ) ) GLOBAL_UNIT_ASSIGNED_CONTEXT ( ( #15190, #10930, #7515 ) ) REPRESENTATION_CONTEXT ( 'NONE', 'WORKASPACE' ) );
#652 = AXIS2_PLACEMENT_3D ( 'NONE', #20653, #18823, #22381 ) ;
#653 = AXIS2_PLACEMENT_3D ( 'NONE', #18782, #3905, #4166 ) ;
#654 = ORIENTED_EDGE ( 'NONE', *, *, #2684, .F. ) ;
#655 = ITEM_DEFINED_TRANSFORMATION ( 'NONE', 'NONE', #19747,  #8005 ) ;
#656 = ADVANCED_FACE ( 'NONE', ( #16980 ), #13077, .F. ) ;
#657 = ORIENTED_EDGE ( 'NONE', *, *, #14862, .T. ) ;
#658 = CARTESIAN_POINT ( 'NONE',  ( 0.000000000000000000, 0.000000000000000000, 0.000000000000000000 ) ) ;
#659 = EDGE_CURVE ( 'NONE', #21366, #3150, #20906, .T. ) ;
#660 = CARTESIAN_POINT ( 'NONE',  ( -9.499999999999790390, -3.086737114213257804, -10.30674201446023375 ) ) ;
#661 = AXIS2_PLACEMENT_3D ( 'NONE', #11705, #19548, #17347 ) ;
#662 = CARTESIAN_POINT ( 'NONE',  ( -41.73082370883258108, -29.50000000000000711, 0.000000000000000000 ) ) ;
#663 = ORIENTED_EDGE ( 'NONE', *, *, #15331, .T. ) ;
#664 = CARTESIAN_POINT ( 'NONE',  ( -40.66734255040736201, -26.56420859267092283, -1.500000000000000000 ) ) ;
#665 = CARTESIAN_POINT ( 'NONE',  ( 0.000000000000000000, 15.50000000000000000, 16.70000000000000284 ) ) ;
#666 = VERTEX_POINT ( 'NONE', #17096 ) ;
#667 = DIRECTION ( 'NONE',  ( 0.000000000000000000, -1.000000000000000000, 0.000000000000000000 ) ) ;
#668 = CARTESIAN_POINT ( 'NONE',  ( 89.12522638709219791, 7.562528597612068045E-15, 0.000000000000000000 ) ) ;
#669 = CARTESIAN_POINT ( 'NONE',  ( 33.99999999999998579, 4.999999999999985789, 10.49999999999999822 ) ) ;
#670 = CARTESIAN_POINT ( 'NONE',  ( 30.68762588338048403, 45.64284848299539732, 0.000000000000000000 ) ) ;
#671 = VERTEX_POINT ( 'NONE', #20543 ) ;
#672 = CARTESIAN_POINT ( 'NONE',  ( -41.00000000000000000, 6.000000000000000888, 11.00000000000000000 ) ) ;
#673 = CARTESIAN_POINT ( 'NONE',  ( -36.00000000000000711, -51.00000000000000711, 0.5000000000000000000 ) ) ;
#674 = ORIENTED_EDGE ( 'NONE', *, *, #22386, .F. ) ;
#675 = EDGE_LOOP ( 'NONE', ( #20908, #21165, #3943, #19400 ) ) ;
#676 = CARTESIAN_POINT ( 'NONE',  ( 2.935661446562616295, -9.035036904803758873, 7.659589141758144315 ) ) ;
#677 = EDGE_CURVE ( 'NONE', #3993, #4215, #21013, .T. ) ;
#678 = VERTEX_POINT ( 'NONE', #13306 ) ;
#679 = EDGE_LOOP ( 'NONE', ( #19832, #3230, #844, #6213, #6205 ) ) ;
#680 = ORIENTED_EDGE ( 'NONE', *, *, #17441, .F. ) ;
#681 = EDGE_CURVE ( 'NONE', #2976, #15778, #14122, .T. ) ;
#682 = ORIENTED_EDGE ( 'NONE', *, *, #20570, .T. ) ;
#683 = ORIENTED_EDGE ( 'NONE', *, *, #3175, .F. ) ;
#684 = EDGE_CURVE ( 'NONE', #411, #21048, #23857, .T. ) ;
#685 = CARTESIAN_POINT ( 'NONE',  ( -45.00000000000001421, 50.99999999999992184, 0.000000000000000000 ) ) ;
#686 = CARTESIAN_POINT ( 'NONE',  ( -6.233975306307046963E-13, 9.127583699786111282, -5.133165578109188054 ) ) ;
#687 = ADVANCED_FACE ( 'NONE', ( #20771 ), #880, .T. ) ;
#688 = EDGE_CURVE ( 'NONE', #12983, #14507, #3818, .T. ) ;
#689 = CYLINDRICAL_SURFACE ( 'NONE', #18467, 50.00000000000000000 ) ;
#690 = ORIENTED_EDGE ( 'NONE', *, *, #14427, .T. ) ;
#691 = CARTESIAN_POINT ( 'NONE',  ( 20.85000000000000853, 15.03999999999999915, 25.00000000000000000 ) ) ;
#692 = DIRECTION ( 'NONE',  ( -1.000000000000000000, -0.000000000000000000, -0.000000000000000000 ) ) ;
#693 = CARTESIAN_POINT ( 'NONE',  ( 5.000000000000000000, 4.685197434473818312, -1.301042606982605321E-15 ) ) ;
#694 = LINE ( 'NONE', #10050, #21251 ) ;
#695 = CARTESIAN_POINT ( 'NONE',  ( 58.00000000000000000, -4.172000000000000597, 5.616230220889771312E-16 ) ) ;
#696 = ORIENTED_EDGE ( 'NONE', *, *, #18309, .T. ) ;
#697 = CARTESIAN_POINT ( 'NONE',  ( -5.871322893123449127, -8.081182679344781405, -6.506742014460233925 ) ) ;
#698 = EDGE_LOOP ( 'NONE', ( #16507, #6423, #6970, #19460 ) ) ;
#699 = CARTESIAN_POINT ( 'NONE',  ( -28.27483331787887266, 41.23752903419610760, 27.00000000000000000 ) ) ;
#700 = DIRECTION ( 'NONE',  ( 0.000000000000000000, 0.000000000000000000, -1.000000000000000000 ) ) ;
#701 = CARTESIAN_POINT ( 'NONE',  ( -2.682529543900285862, 8.255977015246234174, -7.233165578109188587 ) ) ;
#702 = VERTEX_POINT ( 'NONE', #22859 ) ;
#703 = CARTESIAN_POINT ( 'NONE',  ( 30.68762588338048403, 45.64284848299539732, -1.500000000000000000 ) ) ;
#704 = VERTEX_POINT ( 'NONE', #13192 ) ;
#705 = ADVANCED_FACE ( 'NONE', ( #15132 ), #397, .F. ) ;
#706 = EDGE_LOOP ( 'NONE', ( #6726, #22975, #16577, #8092 ) ) ;
#707 = CARTESIAN_POINT ( 'NONE',  ( -6.233975306307046963E-13, 9.127583699786111282, -11.13316557810918894 ) ) ;
#708 = CARTESIAN_POINT ( 'NONE',  ( 8.680847955711007202, 5.912916378492122225E-13, 8.633165578109188942 ) ) ;
#709 = ORIENTED_EDGE ( 'NONE', *, *, #20639, .T. ) ;
#710 = DIRECTION ( 'NONE',  ( -5.198246817781741319E-18, 1.388000771984978914E-17, 1.000000000000000000 ) ) ;
#711 = DIRECTION ( 'NONE',  ( -0.000000000000000000, -0.000000000000000000, -1.000000000000000000 ) ) ;
#712 = EDGE_CURVE ( 'NONE', #10867, #18287, #7477, .T. ) ;
#713 = CARTESIAN_POINT ( 'NONE',  ( -41.99999999999999289, -25.93535998569255341, 27.00000000000000000 ) ) ;
#714 = CARTESIAN_POINT ( 'NONE',  ( 0.000000000000000000, 0.000000000000000000, 0.000000000000000000 ) ) ;
#715 = ADVANCED_FACE ( 'NONE', ( #22496 ), #5772, .F. ) ;
#716 = CIRCLE ( 'NONE', #6156, 1.000000000000000888 ) ;
#717 = CYLINDRICAL_SURFACE ( 'NONE', #14179, 17.87500000001787726 ) ;
#718 = CARTESIAN_POINT ( 'NONE',  ( 8.746907971560217376, -1.213523871515184149, 12.49999999999999289 ) ) ;
#719 = DIRECTION ( 'NONE',  ( 0.000000000000000000, -0.9096319953545137782, -0.4154150130018965936 ) ) ;
#720 = ORIENTED_EDGE ( 'NONE', *, *, #688, .F. ) ;
#721 = VERTEX_POINT ( 'NONE', #7935 ) ;
#722 = DIRECTION ( 'NONE',  ( 1.000000000000000000, 0.000000000000000000, 0.000000000000000000 ) ) ;
#723 = FACE_OUTER_BOUND ( 'NONE', #23290, .T. ) ;
#724 = DIRECTION ( 'NONE',  ( -0.7052211081716915908, 0.7089874389501490404, -0.000000000000000000 ) ) ;
#725 = CARTESIAN_POINT ( 'NONE',  ( 60.03431729618309021, 7.562528597612068045E-15, 0.000000000000000000 ) ) ;
#726 = DIRECTION ( 'NONE',  ( -1.337728473353585242E-16, 1.000000000000000000, -0.000000000000000000 ) ) ;
#727 = FACE_OUTER_BOUND ( 'NONE', #2742, .T. ) ;
#728 = DIRECTION ( 'NONE',  ( 0.000000000000000000, -1.224646799147352221E-16, 1.000000000000000000 ) ) ;
#729 = ORIENTED_EDGE ( 'NONE', *, *, #4251, .F. ) ;
#730 = CARTESIAN_POINT ( 'NONE',  ( 7.685661446562381371, -5.583959896777971110, -13.00674201446023304 ) ) ;
#731 = AXIS2_PLACEMENT_3D ( 'NONE', #7093, #20394, #22131 ) ;
#732 = VERTEX_POINT ( 'NONE', #13445 ) ;
#733 = CARTESIAN_POINT ( 'NONE',  ( 7.685661446562381371, -5.583959896777971110, 11.85958914175814449 ) ) ;
#734 = CARTESIAN_POINT ( 'NONE',  ( -2.935661446561384391, -9.035036904804158553, 10.60674201446023446 ) ) ;
#735 = ORIENTED_EDGE ( 'NONE', *, *, #19095, .F. ) ;
#736 = DIRECTION ( 'NONE',  ( 1.000000000000000000, 2.251221844363938350E-33, -6.162975822039154730E-33 ) ) ;
#737 = DIRECTION ( 'NONE',  ( 0.5654966663575777819, -0.8247505806839220410, 0.000000000000000000 ) ) ;
#738 = CARTESIAN_POINT ( 'NONE',  ( 29.00000000000000355, -29.50000000000000000, -2.224999999999995204 ) ) ;
#739 = FACE_OUTER_BOUND ( 'NONE', #4967, .T. ) ;
#740 = ADVANCED_FACE ( 'NONE', ( #18816 ), #2101, .F. ) ;
#741 = DIRECTION ( 'NONE',  ( 1.000000000000000000, 1.110223024625155594E-14, 0.000000000000000000 ) ) ;
#742 = CARTESIAN_POINT ( 'NONE',  ( 0.9999999999999986677, 1.374779123446053458E-15, -11.22592346138681130 ) ) ;
#743 = PLANE ( 'NONE',  #19572 ) ;
#744 = AXIS2_PLACEMENT_3D ( 'NONE', #8652, #10377, #12195 ) ;
#745 = CARTESIAN_POINT ( 'NONE',  ( 2.935661446562616295, -9.035036904803758873, -3.659589141758142983 ) ) ;
#746 = ORIENTED_EDGE ( 'NONE', *, *, #10848, .F. ) ;
#747 = VERTEX_POINT ( 'NONE', #14052 ) ;
#748 = CARTESIAN_POINT ( 'NONE',  ( 0.000000000000000000, -15.26463740537730729, 9.300885435430041426 ) ) ;
#749 = CARTESIAN_POINT ( 'NONE',  ( 68.18181818181818699, -4.172000000000000597, 5.616230220889771312E-16 ) ) ;
#750 = CARTESIAN_POINT ( 'NONE',  ( -9.499999999999783284, -3.086737114213268018, 11.15958914175814698 ) ) ;
#751 =( LENGTH_UNIT ( ) NAMED_UNIT ( * ) SI_UNIT ( .MILLI., .METRE. ) );
#752 = LINE ( 'NONE', #22588, #4278 ) ;
#753 = ORIENTED_EDGE ( 'NONE', *, *, #6733, .F. ) ;
#754 = CIRCLE ( 'NONE', #12821, 1.500000000000000000 ) ;
#755 = EDGE_CURVE ( 'NONE', #22742, #3887, #21498, .T. ) ;
#756 = DIRECTION ( 'NONE',  ( 0.000000000000000000, 1.000000000000000000, 0.000000000000000000 ) ) ;
#757 = CARTESIAN_POINT ( 'NONE',  ( 2.935661446561383503, 9.035036904804158553, 8.459589141758144137 ) ) ;
#758 = VERTEX_POINT ( 'NONE', #1015 ) ;
#759 = CARTESIAN_POINT ( 'NONE',  ( -9.500000000000211386, 3.086737114211961064, -6.106742014460234458 ) ) ;
#760 = VERTEX_POINT ( 'NONE', #13943 ) ;
#761 = LINE ( 'NONE', #4188, #15587 ) ;
#762 = EDGE_CURVE ( 'NONE', #15778, #2103, #13814, .T. ) ;
#763 = CARTESIAN_POINT ( 'NONE',  ( -6.233975306307045953E-13, 9.127583699786111282, 11.13316557810918894 ) ) ;
#764 = FACE_BOUND ( 'NONE', #23465, .T. ) ;
#765 = DIRECTION ( 'NONE',  ( -1.000000000000000000, -0.000000000000000000, -0.000000000000000000 ) ) ;
#766 = DIRECTION ( 'NONE',  ( 0.000000000000000000, -1.000000000000000000, 0.000000000000000000 ) ) ;
#767 = DIRECTION ( 'NONE',  ( 0.000000000000000000, -0.5000000000000011102, -0.8660254037844380415 ) ) ;
#768 = EDGE_CURVE ( 'NONE', #10954, #4131, #21910, .T. ) ;
#769 = CIRCLE ( 'NONE', #3875, 9.000000000000000000 ) ;
#770 = ORIENTED_EDGE ( 'NONE', *, *, #8119, .T. ) ;
#771 = ORIENTED_EDGE ( 'NONE', *, *, #9688, .T. ) ;
#772 = ITEM_DEFINED_TRANSFORMATION ( 'NONE', 'NONE', #16601,  #8005 ) ;
#773 = ORIENTED_EDGE ( 'NONE', *, *, #14811, .T. ) ;
#774 = DIRECTION ( 'NONE',  ( -1.000000000000000000, -0.000000000000000000, -0.000000000000000000 ) ) ;
#775 = ORIENTED_EDGE ( 'NONE', *, *, #15208, .F. ) ;
#776 = ORIENTED_EDGE ( 'NONE', *, *, #14281, .F. ) ;
#777 = AXIS2_PLACEMENT_3D ( 'NONE', #5867, #22960, #13295 ) ;
#778 = CARTESIAN_POINT ( 'NONE',  ( 28.99999999999998579, -29.49999999999999645, -1.500000000000000000 ) ) ;
#779 = VERTEX_POINT ( 'NONE', #12211 ) ;
#780 = VERTEX_POINT ( 'NONE', #13683 ) ;
#781 = DIRECTION ( 'NONE',  ( 1.000000000000000000, 8.881784197001252323E-16, 0.000000000000000000 ) ) ;
#782 = DIRECTION ( 'NONE',  ( 0.000000000000000000, 1.000000000000000000, 0.000000000000000000 ) ) ;
#783 = DIRECTION ( 'NONE',  ( -0.8191520442889927978, -5.579613378627572123E-14, -0.5735764363510448272 ) ) ;
#784 = DIRECTION ( 'NONE',  ( -0.000000000000000000, -0.000000000000000000, -1.000000000000000000 ) ) ;
#785 = ORIENTED_EDGE ( 'NONE', *, *, #16933, .F. ) ;
#786 = DIRECTION ( 'NONE',  ( -0.5000000000000002220, 0.8660254037844384856, 0.000000000000000000 ) ) ;
#787 = EDGE_CURVE ( 'NONE', #11482, #5195, #15888, .T. ) ;
#788 = CARTESIAN_POINT ( 'NONE',  ( 89.12522638709219791, 7.562528597612068045E-15, 0.000000000000000000 ) ) ;
#789 = EDGE_CURVE ( 'NONE', #7728, #5147, #13740, .T. ) ;
#790 = CARTESIAN_POINT ( 'NONE',  ( 5.871322893123448239, 8.081182679344781405, -4.359589141758143604 ) ) ;
#791 = ORIENTED_EDGE ( 'NONE', *, *, #13348, .F. ) ;
#792 = ORIENTED_EDGE ( 'NONE', *, *, #2605, .T. ) ;
#793 = CARTESIAN_POINT ( 'NONE',  ( 9.500000000000209610, -3.086737114211962396, 9.959589141758145914 ) ) ;
#794 = ORIENTED_EDGE ( 'NONE', *, *, #18251, .T. ) ;
#795 = AXIS2_PLACEMENT_3D ( 'NONE', #13930, #21617, #4783 ) ;
#796 = EDGE_LOOP ( 'NONE', ( #16401, #12059, #620, #14476, #16004 ) ) ;
#797 = ORIENTED_EDGE ( 'NONE', *, *, #22985, .F. ) ;
#798 = ORIENTED_EDGE ( 'NONE', *, *, #5110, .T. ) ;
#799 = CARTESIAN_POINT ( 'NONE',  ( 42.00000000000000000, 26.82133436441678853, 11.00000000000000000 ) ) ;
#800 = DIRECTION ( 'NONE',  ( 0.000000000000000000, -1.000000000000000000, 0.000000000000000000 ) ) ;
#801 = CARTESIAN_POINT ( 'NONE',  ( 9.500000000000000000, 6.470877716354879437E-13, 7.206742014460234103 ) ) ;
#802 = ORIENTED_EDGE ( 'NONE', *, *, #12261, .F. ) ;
#803 = CARTESIAN_POINT ( 'NONE',  ( -16.18147534945000032, -6.260849737139247750, 7.148624562014530781 ) ) ;
#804 = DIRECTION ( 'NONE',  ( 0.000000000000000000, 0.9898214418809322401, 0.1423148382732887796 ) ) ;
#805 = DIRECTION ( 'NONE',  ( -0.000000000000000000, -0.000000000000000000, -1.000000000000000000 ) ) ;
#806 = ORIENTED_EDGE ( 'NONE', *, *, #11080, .F. ) ;
#807 = DIRECTION ( 'NONE',  ( -0.000000000000000000, -0.000000000000000000, -1.000000000000000000 ) ) ;
#808 = AXIS2_PLACEMENT_3D ( 'NONE', #4669, #4301, #12072 ) ;
#809 = AXIS2_PLACEMENT_3D ( 'NONE', #22982, #8323, #7950 ) ;
#810 = ORIENTED_EDGE ( 'NONE', *, *, #4959, .F. ) ;
#811 = CARTESIAN_POINT ( 'NONE',  ( 4.489900896931573904, 0.000000000000000000, 0.000000000000000000 ) ) ;
#812 = SURFACE_STYLE_USAGE ( .BOTH. , #11531 ) ;
#813 = LINE ( 'NONE', #4975, #3726 ) ;
#814 = DIRECTION ( 'NONE',  ( -0.000000000000000000, -0.000000000000000000, 1.000000000000000000 ) ) ;
#815 = EDGE_CURVE ( 'NONE', #11364, #23753, #21137, .T. ) ;
#816 = CARTESIAN_POINT ( 'NONE',  ( 5.365059087798939252, 7.384370330707087149, -4.933165578109186988 ) ) ;
#817 = EDGE_CURVE ( 'NONE', #20489, #21814, #117, .T. ) ;
#818 = CARTESIAN_POINT ( 'NONE',  ( 68.76159002345582394, -5.000000000000000888, 6.123233995736776143E-16 ) ) ;
#819 = ORIENTED_EDGE ( 'NONE', *, *, #399, .F. ) ;
#820 = ORIENTED_EDGE ( 'NONE', *, *, #6931, .T. ) ;
#821 = CARTESIAN_POINT ( 'NONE',  ( 6.222797240145152671E-13, -9.127583699786111282, 10.13316557810918894 ) ) ;
#822 = ORIENTED_EDGE ( 'NONE', *, *, #9732, .F. ) ;
#823 = CARTESIAN_POINT ( 'NONE',  ( 27.88015375556323505, 31.77618558084328271, 10.22831690717757702 ) ) ;
#824 = DIRECTION ( 'NONE',  ( -0.5735764363510519326, 0.8191520442889876907, 1.003171929053519816E-16 ) ) ;
#825 = VECTOR ( 'NONE', #21325, 1000.000000000000000 ) ;
#826 = ORIENTED_EDGE ( 'NONE', *, *, #3707, .T. ) ;
#827 = CARTESIAN_POINT ( 'NONE',  ( -29.00000000000000000, 29.49999999999999645, 11.50000000000000000 ) ) ;
#828 = CARTESIAN_POINT ( 'NONE',  ( 7.751944208201821063, -4.001916517787171834, 12.50000000000000711 ) ) ;
#829 = CARTESIAN_POINT ( 'NONE',  ( 62.36363636363636687, 7.491529369508391930E-15, 0.000000000000000000 ) ) ;
#830 = DIRECTION ( 'NONE',  ( -5.501724186093582121E-16, 1.000000000000000000, 0.000000000000000000 ) ) ;
#831 = VERTEX_POINT ( 'NONE', #23222 ) ;
#832 = CYLINDRICAL_SURFACE ( 'NONE', #16173, 6.050000000006050982 ) ;
#833 = DIRECTION ( 'NONE',  ( -0.000000000000000000, -1.000000000000000000, -0.000000000000000000 ) ) ;
#834 = EDGE_CURVE ( 'NONE', #21352, #8760, #14170, .T. ) ;
#835 = CARTESIAN_POINT ( 'NONE',  ( -31.74999999999995737, 0.000000000000000000, 0.000000000000000000 ) ) ;
#836 = CARTESIAN_POINT ( 'NONE',  ( 9.500000000000000000, 6.470877716354879437E-13, -9.206742014460234103 ) ) ;
#837 = LINE ( 'NONE', #17056, #14124 ) ;
#838 = CYLINDRICAL_SURFACE ( 'NONE', #3638, 11.23082370883260417 ) ;
#839 = CARTESIAN_POINT ( 'NONE',  ( -28.99999999999998579, -29.50000000000000711, -3.000000000000000000 ) ) ;
#840 = ADVANCED_FACE ( 'NONE', ( #11965, #19433 ), #4926, .T. ) ;
#841 = ORIENTED_EDGE ( 'NONE', *, *, #22771, .T. ) ;
#842 = CARTESIAN_POINT ( 'NONE',  ( -9.500000000000211386, 3.086737114211961064, -12.10674201446023091 ) ) ;
#843 = EDGE_CURVE ( 'NONE', #19427, #5371, #11846, .T. ) ;
#844 = ORIENTED_EDGE ( 'NONE', *, *, #18637, .T. ) ;
#845 = ORIENTED_EDGE ( 'NONE', *, *, #20971, .T. ) ;
#846 = CARTESIAN_POINT ( 'NONE',  ( -9.500000000000000000, -6.482511860946779655E-13, 9.059589141758143782 ) ) ;
#847 = CARTESIAN_POINT ( 'NONE',  ( -41.00000000000000000, -6.000000000000000888, 11.00000000000000000 ) ) ;
#848 = ORIENTED_EDGE ( 'NONE', *, *, #22737, .T. ) ;
#849 = SHAPE_REPRESENTATION_RELATIONSHIP ( 'NONE' , 'NONE' ,  #7043, #16009 ) ;
#850 = DIRECTION ( 'NONE',  ( -0.000000000000000000, -0.000000000000000000, -1.000000000000000000 ) ) ;
#851 = CARTESIAN_POINT ( 'NONE',  ( -20.84999999999999787, 16.67999999999985405, 13.00000000000000178 ) ) ;
#852 = SHAPE_REPRESENTATION ( 'Oil seal', ( #8005 ), #1445 ) ;
#853 = CIRCLE ( 'NONE', #13299, 1.000000000000000888 ) ;
#854 = DIRECTION ( 'NONE',  ( 0.9160001545545232160, 0.4011779117250717785, 0.000000000000000000 ) ) ;
#855 = DIRECTION ( 'NONE',  ( -0.000000000000000000, -0.000000000000000000, -1.000000000000000000 ) ) ;
#856 = DIRECTION ( 'NONE',  ( 0.000000000000000000, -1.000000000000000000, 0.000000000000000000 ) ) ;
#857 = PRODUCT ( 'Assembly Idle gear', 'Assembly Idle gear', '', ( #11022 ) ) ;
#858 = AXIS2_PLACEMENT_3D ( 'NONE', #13331, #538, #11614 ) ;
#859 = CARTESIAN_POINT ( 'NONE',  ( -7.685661446562381371, 5.583959896777970222, -2.859589141758144493 ) ) ;
#860 = ORIENTED_EDGE ( 'NONE', *, *, #16308, .F. ) ;
#861 = CARTESIAN_POINT ( 'NONE',  ( -42.00000000000000000, -6.000000000000000888, 11.00000000000000000 ) ) ;
#862 = ORIENTED_EDGE ( 'NONE', *, *, #3081, .F. ) ;
#863 = DIRECTION ( 'NONE',  ( -0.5735764363510517105, -0.8191520442889879128, 0.000000000000000000 ) ) ;
#864 = FACE_OUTER_BOUND ( 'NONE', #3660, .T. ) ;
#865 = CARTESIAN_POINT ( 'NONE',  ( 11.50000000000000000, -17.86986844953241516, -0.4282833139928948207 ) ) ;
#866 = DIRECTION ( 'NONE',  ( -0.000000000000000000, -0.000000000000000000, 1.000000000000000000 ) ) ;
#867 = DIRECTION ( 'NONE',  ( -1.000000000000000000, 0.000000000000000000, 0.000000000000000000 ) ) ;
#868 = ORIENTED_EDGE ( 'NONE', *, *, #22214, .F. ) ;
#869 = EDGE_CURVE ( 'NONE', #5396, #14991, #8668, .T. ) ;
#870 = DIRECTION ( 'NONE',  ( 1.000000000000000000, -2.600433232233976523E-16, 0.000000000000000000 ) ) ;
#871 = DIRECTION ( 'NONE',  ( -0.000000000000000000, -0.000000000000000000, -1.000000000000000000 ) ) ;
#872 = EDGE_CURVE ( 'NONE', #15778, #2976, #11765, .T. ) ;
#873 = ORIENTED_EDGE ( 'NONE', *, *, #9298, .T. ) ;
#874 = CARTESIAN_POINT ( 'NONE',  ( 2.935661446561383503, 9.035036904804158553, -7.606742014460233570 ) ) ;
#875 = AXIS2_PLACEMENT_3D ( 'NONE', #11643, #9445, #19001 ) ;
#876 = ORIENTED_EDGE ( 'NONE', *, *, #14081, .T. ) ;
#877 = AXIS2_PLACEMENT_3D ( 'NONE', #20362, #14746, #3776 ) ;
#878 = CARTESIAN_POINT ( 'NONE',  ( 9.500000000000000000, 6.470877716354879437E-13, -6.059589141758143782 ) ) ;
#879 = CARTESIAN_POINT ( 'NONE',  ( 8.680847955711199049, -2.820578480813074496, 10.53316557810918752 ) ) ;
#880 = CONICAL_SURFACE ( 'NONE', #23083, 4.172000000000008590, 0.9599310885968742602 ) ;
#881 = CIRCLE ( 'NONE', #14887, 13.72592346138681130 ) ;
#882 = CIRCLE ( 'NONE', #14871, 5.000000000000007994 ) ;
#883 = PLANE ( 'NONE',  #8037 ) ;
#884 = AXIS2_PLACEMENT_3D ( 'NONE', #22876, #11979, #2243 ) ;
#885 = AXIS2_PLACEMENT_3D ( 'NONE', #18229, #8575, #17984 ) ;
#886 = VERTEX_POINT ( 'NONE', #10737 ) ;
#887 = ORIENTED_EDGE ( 'NONE', *, *, #1639, .T. ) ;
#888 = DIRECTION ( 'NONE',  ( -0.7071067811865489050, 8.659560562354950115E-17, 0.7071067811865462405 ) ) ;
#889 = CARTESIAN_POINT ( 'NONE',  ( 2.935661446561383503, 9.035036904804158553, -11.60674201446023268 ) ) ;
#890 = ORIENTED_EDGE ( 'NONE', *, *, #7196, .T. ) ;
#891 = VERTEX_POINT ( 'NONE', #1602 ) ;
#892 = CARTESIAN_POINT ( 'NONE',  ( -5.614908434072717114, -7.307052314572652918, -12.29292215563023483 ) ) ;
#893 = CIRCLE ( 'NONE', #14139, 9.999999999999998224 ) ;
#894 = EDGE_CURVE ( 'NONE', #22006, #22524, #7859, .T. ) ;
#895 = CIRCLE ( 'NONE', #5571, 5.000000000000007994 ) ;
#896 = CYLINDRICAL_SURFACE ( 'NONE', #9627, 49.99999999999998579 ) ;
#897 = TOROIDAL_SURFACE ( 'NONE', #14515, 21.85000000000000142, 1.000000000000000000 ) ;
#898 = VERTEX_POINT ( 'NONE', #6975 ) ;
#899 = CARTESIAN_POINT ( 'NONE',  ( -9.999999999999998224, 0.000000000000000000, 15.50000000000000000 ) ) ;
#900 = AXIS2_PLACEMENT_3D ( 'NONE', #7042, #870, #23670 ) ;
#901 = CONICAL_SURFACE ( 'NONE', #20383, 5.000000000000007994, 0.9599310885968855844 ) ;
#902 = EDGE_CURVE ( 'NONE', #17696, #14019, #8899, .T. ) ;
#903 = ORIENTED_EDGE ( 'NONE', *, *, #21850, .F. ) ;
#904 = CARTESIAN_POINT ( 'NONE',  ( 0.000000000000000000, 0.000000000000000000, 11.00000000000000000 ) ) ;
#905 = ADVANCED_FACE ( 'NONE', ( #1846 ), #14401, .F. ) ;
#906 = AXIS2_PLACEMENT_3D ( 'NONE', #13168, #22574, #13282 ) ;
#907 = CARTESIAN_POINT ( 'NONE',  ( -29.00000000000000000, 29.49999999999999645, 12.00000000000000000 ) ) ;
#908 = CARTESIAN_POINT ( 'NONE',  ( 0.000000000000000000, 1.377380391735521048E-15, -11.24716442891539714 ) ) ;
#909 = DIRECTION ( 'NONE',  ( -1.000000000000000000, -1.224606353822377258E-16, -0.000000000000000000 ) ) ;
#910 = VERTEX_POINT ( 'NONE', #21750 ) ;
#911 = DIRECTION ( 'NONE',  ( -0.5735764363510517105, -0.8191520442889879128, 0.000000000000000000 ) ) ;
#912 = CARTESIAN_POINT ( 'NONE',  ( -7.685661446562381371, 5.583959896777970222, -4.859589141758143604 ) ) ;
#913 = EDGE_LOOP ( 'NONE', ( #1338, #8471, #1416 ) ) ;
#914 = CARTESIAN_POINT ( 'NONE',  ( 9.499999999999790390, 3.086737114213260025, 10.15958914175814520 ) ) ;
#915 = AXIS2_PLACEMENT_3D ( 'NONE', #442, #15301, #22902 ) ;
#916 = ORIENTED_EDGE ( 'NONE', *, *, #4388, .T. ) ;
#917 = AXIS2_PLACEMENT_3D ( 'NONE', #94, #16678, #11144 ) ;
#918 = ORIENTED_EDGE ( 'NONE', *, *, #23641, .F. ) ;
#919 = CIRCLE ( 'NONE', #14538, 49.00000000000000000 ) ;
#920 = ORIENTED_EDGE ( 'NONE', *, *, #15760, .T. ) ;
#921 = EDGE_LOOP ( 'NONE', ( #1587, #18465, #20658, #20990 ) ) ;
#922 = DIRECTION ( 'NONE',  ( -0.000000000000000000, -0.000000000000000000, -1.000000000000000000 ) ) ;
#923 = CARTESIAN_POINT ( 'NONE',  ( -8.680847955710813579, -2.820578480814258437, -3.733165578109188587 ) ) ;
#924 = AXIS2_PLACEMENT_3D ( 'NONE', #5364, #24025, #7646 ) ;
#925 = DIRECTION ( 'NONE',  ( 0.000000000000000000, 0.000000000000000000, 1.000000000000000000 ) ) ;
#926 = CARTESIAN_POINT ( 'NONE',  ( 41.00000000000000000, 5.999999999999986677, 9.500000000000000000 ) ) ;
#927 = ORIENTED_EDGE ( 'NONE', *, *, #22597, .T. ) ;
#928 = CARTESIAN_POINT ( 'NONE',  ( -15.78970982176773319, -5.581464347350857835, -7.700125654604357273 ) ) ;
#929 = CARTESIAN_POINT ( 'NONE',  ( 90.00000000000000000, 5.616230220889761452E-16, -4.171999999999999709 ) ) ;
#930 = EDGE_CURVE ( 'NONE', #3367, #22006, #21537, .T. ) ;
#931 = CARTESIAN_POINT ( 'NONE',  ( 1.999999999999994449, -45.00000000000000000, 0.000000000000000000 ) ) ;
#932 = ORIENTED_EDGE ( 'NONE', *, *, #12883, .F. ) ;
#933 = FACE_OUTER_BOUND ( 'NONE', #2326, .T. ) ;
#934 = DIRECTION ( 'NONE',  ( 0.000000000000000000, -1.000000000000000000, 0.000000000000000000 ) ) ;
#935 = AXIS2_PLACEMENT_3D ( 'NONE', #16802, #13032, #13266 ) ;
#936 = DIRECTION ( 'NONE',  ( -1.000000000000000000, -0.000000000000000000, -0.000000000000000000 ) ) ;
#937 = LINE ( 'NONE', #15814, #20706 ) ;
#938 = AXIS2_PLACEMENT_3D ( 'NONE', #22239, #12943, #5510 ) ;
#939 = VECTOR ( 'NONE', #9916, 1000.000000000000000 ) ;
#940 = CARTESIAN_POINT ( 'NONE',  ( 77.78386452199872281, 6.123233995736675563E-16, -5.000000000000007994 ) ) ;
#941 = DIRECTION ( 'NONE',  ( -0.000000000000000000, -0.000000000000000000, -1.000000000000000000 ) ) ;
#942 = CIRCLE ( 'NONE', #1388, 4.172000000000008590 ) ;
#943 = CARTESIAN_POINT ( 'NONE',  ( 7.022953521755574080, -5.102474405759714671, -8.433165578109187877 ) ) ;
#944 = VECTOR ( 'NONE', #4341, 1000.000000000000000 ) ;
#945 = DIRECTION ( 'NONE',  ( -0.000000000000000000, -0.000000000000000000, -1.000000000000000000 ) ) ;
#946 = ORIENTED_EDGE ( 'NONE', *, *, #19577, .F. ) ;
#947 = EDGE_LOOP ( 'NONE', ( #13196, #14104, #14559, #19389 ) ) ;
#948 = AXIS2_PLACEMENT_3D ( 'NONE', #20864, #13152, #20977 ) ;
#949 = CARTESIAN_POINT ( 'NONE',  ( -6.233975306307046963E-13, 9.127583699786111282, 9.133165578109188942 ) ) ;
#950 = EDGE_LOOP ( 'NONE', ( #1693, #8351, #298, #18257 ) ) ;
#951 = CARTESIAN_POINT ( 'NONE',  ( 693.7818939062881327, 843.4837211537981148, 1290.481724745928432 ) ) ;
#952 = DIRECTION ( 'NONE',  ( 1.000000000000000000, 0.000000000000000000, 0.000000000000000000 ) ) ;
#953 = ORIENTED_EDGE ( 'NONE', *, *, #12676, .F. ) ;
#954 = FACE_BOUND ( 'NONE', #5585, .T. ) ;
#955 = LINE ( 'NONE', #8125, #3358 ) ;
#956 = COLOUR_RGB ( '',0.7921568627450980005, 0.8196078431372548767, 0.9333333333333333481 ) ;
#957 = LINE ( 'NONE', #14005, #19246 ) ;
#958 = CARTESIAN_POINT ( 'NONE',  ( 0.000000000000000000, -8.772759796005278332, 7.720943453482002283 ) ) ;
#959 = FACE_OUTER_BOUND ( 'NONE', #22292, .T. ) ;
#960 = ORIENTED_EDGE ( 'NONE', *, *, #478, .F. ) ;
#961 = ADVANCED_FACE ( 'NONE', ( #7323 ), #5040, .F. ) ;
#962 = AXIS2_PLACEMENT_3D ( 'NONE', #19930, #8691, #23609 ) ;
#963 = EDGE_CURVE ( 'NONE', #1596, #21975, #18029, .T. ) ;
#964 = AXIS2_PLACEMENT_3D ( 'NONE', #3575, #16384, #23839 ) ;
#965 = EDGE_LOOP ( 'NONE', ( #1076, #18624, #5480, #18490, #21269 ) ) ;
#966 = CARTESIAN_POINT ( 'NONE',  ( 0.000000000000000000, -45.00000000000000000, 27.00000000000000000 ) ) ;
#967 = AXIS2_PLACEMENT_3D ( 'NONE', #15842, #14011, #1206 ) ;
#968 = CARTESIAN_POINT ( 'NONE',  ( -6.153822176767817416E-13, 9.500000000000000000, -2.846377359933665030 ) ) ;
#969 = ORIENTED_EDGE ( 'NONE', *, *, #16996, .T. ) ;
#970 = DIRECTION ( 'NONE',  ( -1.000000000000000000, 0.000000000000000000, 0.000000000000000000 ) ) ;
#971 = DIRECTION ( 'NONE',  ( 0.000000000000000000, -1.000000000000000000, 0.000000000000000000 ) ) ;
#972 = CARTESIAN_POINT ( 'NONE',  ( 90.00000000000000000, 0.000000000000000000, 4.171999999999999709 ) ) ;
#973 = CARTESIAN_POINT ( 'NONE',  ( -23.85000000000000497, 15.03999999999999915, -27.00000000000000000 ) ) ;
#974 = ORIENTED_EDGE ( 'NONE', *, *, #5929, .T. ) ;
#975 = CARTESIAN_POINT ( 'NONE',  ( 6.809999908187194197E-13, -9.988891130263535700, -12.70674201446023410 ) ) ;
#976 = CIRCLE ( 'NONE', #13035, 4.999999999999997335 ) ;
#977 = VERTEX_POINT ( 'NONE', #9155 ) ;
#978 = VERTEX_POINT ( 'NONE', #11083 ) ;
#979 = CARTESIAN_POINT ( 'NONE',  ( 6.809999908187194197E-13, -9.988891130263535700, 3.559589141758143338 ) ) ;
#980 = DIRECTION ( 'NONE',  ( 0.000000000000000000, 1.000000000000000000, 0.000000000000000000 ) ) ;
#981 = CIRCLE ( 'NONE', #16926, 1.000000000000000888 ) ;
#982 = ORIENTED_EDGE ( 'NONE', *, *, #12348, .T. ) ;
#983 = DIRECTION ( 'NONE',  ( 0.000000000000000000, -0.5000000000000013323, -0.8660254037844379305 ) ) ;
#984 = EDGE_CURVE ( 'NONE', #18951, #10181, #23934, .T. ) ;
#985 = AXIS2_PLACEMENT_3D ( 'NONE', #13641, #470, #7655 ) ;
#986 = DIRECTION ( 'NONE',  ( -0.000000000000000000, -0.000000000000000000, 1.000000000000000000 ) ) ;
#987 = CARTESIAN_POINT ( 'NONE',  ( 0.000000000000000000, -2.110835303355205639, -14.05523051341068097 ) ) ;
#988 = EDGE_CURVE ( 'NONE', #8523, #18614, #3318, .T. ) ;
#989 = DIRECTION ( 'NONE',  ( 0.000000000000000000, 0.000000000000000000, -1.000000000000000000 ) ) ;
#990 = CARTESIAN_POINT ( 'NONE',  ( 11.49999999999999822, -15.26463740537730551, 9.300885435430041426 ) ) ;
#991 = ADVANCED_FACE ( 'NONE', ( #16125 ), #17225, .T. ) ;
#992 = EDGE_CURVE ( 'NONE', #20705, #4244, #3436, .T. ) ;
#993 = EDGE_CURVE ( 'NONE', #11156, #14408, #6731, .T. ) ;
#994 = ORIENTED_EDGE ( 'NONE', *, *, #19149, .F. ) ;
#995 = ORIENTED_EDGE ( 'NONE', *, *, #13482, .T. ) ;
#996 = CARTESIAN_POINT ( 'NONE',  ( 0.000000000000000000, 0.000000000000000000, 27.00000000000000000 ) ) ;
#997 = CARTESIAN_POINT ( 'NONE',  ( 59.45454545454545325, -4.172000000000000597, 5.616230220889771312E-16 ) ) ;
#999 = DIRECTION ( 'NONE',  ( -1.000000000000000000, 0.000000000000000000, 0.000000000000000000 ) ) ;
#998 = VECTOR ( 'NONE', #5419, 1000.000000000000000 ) ;
#1000 = DIRECTION ( 'NONE',  ( 0.000000000000000000, -0.000000000000000000, -1.000000000000000000 ) ) ;
#1001 = CIRCLE ( 'NONE', #11092, 10.50249999999999950 ) ;
#1002 = LINE ( 'NONE', #2950, #14791 ) ;
#1003 = EDGE_LOOP ( 'NONE', ( #7605, #44, #18685, #22956 ) ) ;
#1004 = AXIS2_PLACEMENT_3D ( 'NONE', #17938, #1109, #3055 ) ;
#1005 = DIRECTION ( 'NONE',  ( -1.000000000000000000, 0.000000000000000000, -0.000000000000000000 ) ) ;
#1006 = AXIS2_PLACEMENT_3D ( 'NONE', #20730, #5740, #11431 ) ;
#1007=STYLED_ITEM('',(#24155),#2970);
#1008 = VERTEX_POINT ( 'NONE', #5496 ) ;
#1009 = CARTESIAN_POINT ( 'NONE',  ( 64.69295543108962931, -4.999999999999989342, 0.000000000000000000 ) ) ;
#1010 = VERTEX_POINT ( 'NONE', #10957 ) ;
#1011 = CARTESIAN_POINT ( 'NONE',  ( 8.680847955711007202, 5.912916378492122225E-13, 4.633165578109188942 ) ) ;
#1012 = CARTESIAN_POINT ( 'NONE',  ( 0.000000000000000000, 0.000000000000000000, -12.50000000000000000 ) ) ;
#1013 = SHAPE_REPRESENTATION ( 'Drive End Plate', ( #8005 ), #15828 ) ;
#1014 = EDGE_CURVE ( 'NONE', #4702, #7988, #1279, .T. ) ;
#1015 = CARTESIAN_POINT ( 'NONE',  ( -23.90000000000000213, -29.49999999999999645, 11.50000000000000000 ) ) ;
#1016 = DIRECTION ( 'NONE',  ( -1.000000000000000000, -0.000000000000000000, -0.000000000000000000 ) ) ;
#1017 = CARTESIAN_POINT ( 'NONE',  ( 5.871322893124551356, -8.081182679343980269, 5.759589141758143960 ) ) ;
#1018 = VECTOR ( 'NONE', #7762, 1000.000000000000000 ) ;
#1019 = EDGE_CURVE ( 'NONE', #16520, #17900, #9810, .T. ) ;
#1020 = VECTOR ( 'NONE', #7871, 1000.000000000000000 ) ;
#1021 = CONTEXT_DEPENDENT_SHAPE_REPRESENTATION ( #6844, #19221 ) ;
#1022 = ORIENTED_EDGE ( 'NONE', *, *, #19910, .T. ) ;
#1023 = DIRECTION ( 'NONE',  ( 0.000000000000000000, 0.5406408174555986657, -0.8412535328311804284 ) ) ;
#1025 = EDGE_CURVE ( 'NONE', #23079, #8542, #15656, .T. ) ;
#1024 = AXIS2_PLACEMENT_3D ( 'NONE', #17998, #1293, #4604 ) ;
#1026 = AXIS2_PLACEMENT_3D ( 'NONE', #2990, #4588, #23114 ) ;
#1027 = CARTESIAN_POINT ( 'NONE',  ( -9.499999999999790390, -3.086737114213257804, -11.15958914175814520 ) ) ;
#1028 = ORIENTED_EDGE ( 'NONE', *, *, #11588, .F. ) ;
#1029 = ORIENTED_EDGE ( 'NONE', *, *, #18657, .F. ) ;
#1030 = DIRECTION ( 'NONE',  ( -0.9160001545545232160, -0.4011779117250717785, 0.000000000000000000 ) ) ;
#1031 = FACE_BOUND ( 'NONE', #499, .T. ) ;
#1032 = ORIENTED_EDGE ( 'NONE', *, *, #12208, .F. ) ;
#1033 = CARTESIAN_POINT ( 'NONE',  ( 1.041919733032276918, 45.00000000000000000, 0.000000000000000000 ) ) ;
#1034 = ORIENTED_EDGE ( 'NONE', *, *, #17512, .T. ) ;
#1035 = DIRECTION ( 'NONE',  ( -0.000000000000000000, 1.000000000000000000, -0.000000000000000000 ) ) ;
#1036 = AXIS2_PLACEMENT_3D ( 'NONE', #1200, #8747, #23760 ) ;
#1037 = DIRECTION ( 'NONE',  ( 0.000000000000000000, 0.000000000000000000, 1.000000000000000000 ) ) ;
#1038 = DIRECTION ( 'NONE',  ( 0.000000000000000000, -1.000000000000000000, 0.000000000000000000 ) ) ;
#1039 = CARTESIAN_POINT ( 'NONE',  ( 64.69295543108962931, -9.244463733058732095E-30, 5.000000000000007994 ) ) ;
#1040 = VECTOR ( 'NONE', #5115, 1000.000000000000000 ) ;
#1041 = DIRECTION ( 'NONE',  ( 0.000000000000000000, 0.2817325568414237313, 0.9594929736144991450 ) ) ;
#1042 = ORIENTED_EDGE ( 'NONE', *, *, #15791, .F. ) ;
#1043 = CARTESIAN_POINT ( 'NONE',  ( -6.250000000000000888, 10.82531754730548279, 2.500000000000000000 ) ) ;
#1044 = CARTESIAN_POINT ( 'NONE',  ( -41.00000000000000000, -5.000000000000000888, 10.49999999999999822 ) ) ;
#1045 = DIRECTION ( 'NONE',  ( 0.000000000000000000, -1.000000000000000000, 0.000000000000000000 ) ) ;
#1046 = AXIS2_PLACEMENT_3D ( 'NONE', #5008, #14371, #21828 ) ;
#1047 = CARTESIAN_POINT ( 'NONE',  ( -2.935661446562617183, 9.035036904803758873, 4.659589141758143427 ) ) ;
#1048 = ORIENTED_EDGE ( 'NONE', *, *, #6379, .T. ) ;
#1049 = ORIENTED_EDGE ( 'NONE', *, *, #15730, .F. ) ;
#1050 = ORIENTED_EDGE ( 'NONE', *, *, #8866, .T. ) ;
#1051 = ORIENTED_EDGE ( 'NONE', *, *, #3127, .F. ) ;
#1052 = DIRECTION ( 'NONE',  ( 0.000000000000000000, 0.000000000000000000, 1.000000000000000000 ) ) ;
#1053 = AXIS2_PLACEMENT_3D ( 'NONE', #14051, #2596, #23348 ) ;
#1054 = ADVANCED_FACE ( 'NONE', ( #22347 ), #18785, .F. ) ;
#1055 = CARTESIAN_POINT ( 'NONE',  ( 9.499999999999799272, 3.086737114213245370, 7.306742014460232859 ) ) ;
#1056 = CARTESIAN_POINT ( 'NONE',  ( 42.00000000000000000, 4.999999999999986677, 10.49999999999999822 ) ) ;
#1057 = CIRCLE ( 'NONE', #17789, 5.099999999999996980 ) ;
#1058 = EDGE_LOOP ( 'NONE', ( #23023, #11672 ) ) ;
#1059 = CARTESIAN_POINT ( 'NONE',  ( 23.00000000000000000, 14.21257171757157955, -0.08908218613038007549 ) ) ;
#1060 = DIRECTION ( 'NONE',  ( 4.613626265895763066E-16, 1.000000000000000000, 0.000000000000000000 ) ) ;
#1061 = ORIENTED_EDGE ( 'NONE', *, *, #3350, .T. ) ;
#1062 = PLANE ( 'NONE',  #12306 ) ;
#1063 = AXIS2_PLACEMENT_3D ( 'NONE', #9729, #17186, #15480 ) ;
#1064 = DIRECTION ( 'NONE',  ( -0.000000000000000000, -0.000000000000000000, -1.000000000000000000 ) ) ;
#1065 = CARTESIAN_POINT ( 'NONE',  ( 2.935661446561383503, 9.035036904804158553, 5.606742014460233570 ) ) ;
#1066 = CARTESIAN_POINT ( 'NONE',  ( -30.44534269664590198, -40.40463133211081015, 27.00000000000000000 ) ) ;
#1067 = CARTESIAN_POINT ( 'NONE',  ( -5.871322893124554021, 8.081182679343978492, 4.759589141758143960 ) ) ;
#1068 = DIRECTION ( 'NONE',  ( 0.000000000000000000, -1.000000000000000000, 0.000000000000000000 ) ) ;
#1069 = DIRECTION ( 'NONE',  ( 0.000000000000000000, 0.000000000000000000, 1.000000000000000000 ) ) ;
#1070 = CARTESIAN_POINT ( 'NONE',  ( 2.682529543900284974, -8.255977015246234174, -10.23316557810918859 ) ) ;
#1071 = ADVANCED_FACE ( 'NONE', ( #13164 ), #19610, .T. ) ;
#1072 = CIRCLE ( 'NONE', #3389, 6.050000000006049206 ) ;
#1073 = ORIENTED_EDGE ( 'NONE', *, *, #12807, .T. ) ;
#1074 = AXIS2_PLACEMENT_3D ( 'NONE', #10333, #12286, #19386 ) ;
#1075 = FACE_OUTER_BOUND ( 'NONE', #6085, .T. ) ;
#1076 = ORIENTED_EDGE ( 'NONE', *, *, #16220, .T. ) ;
#1077 = ORIENTED_EDGE ( 'NONE', *, *, #21532, .F. ) ;
#1078 = EDGE_CURVE ( 'NONE', #780, #10236, #16463, .T. ) ;
#1079 = CARTESIAN_POINT ( 'NONE',  ( -2.682529543899159208, -8.255977015246598327, 4.033165578109189298 ) ) ;
#1080 = PRODUCT_DEFINITION_SHAPE ( 'NONE', 'NONE',  #24113 ) ;
#1081 = ORIENTED_EDGE ( 'NONE', *, *, #23581, .T. ) ;
#1082 = DIRECTION ( 'NONE',  ( 0.000000000000000000, 0.5783365841231422610, -0.8157982565958178389 ) ) ;
#1083 = CARTESIAN_POINT ( 'NONE',  ( 7.685661446561619314, 5.583959896779020049, -11.40674201446023517 ) ) ;
#1084 = ORIENTED_EDGE ( 'NONE', *, *, #1377, .T. ) ;
#1085 = DIRECTION ( 'NONE',  ( 0.000000000000000000, 0.000000000000000000, -1.000000000000000000 ) ) ;
#1086 = CARTESIAN_POINT ( 'NONE',  ( 5.871322893124553133, -8.081182679343980269, -11.75958914175814485 ) ) ;
#1087 = UNCERTAINTY_MEASURE_WITH_UNIT (LENGTH_MEASURE( 1.000000000000000082E-05 ), #10598, 'distance_accuracy_value', 'NONE');
#1088 = CARTESIAN_POINT ( 'NONE',  ( -35.99999999999995026, 59.99999999999998579, 12.50000000000000000 ) ) ;
#1089 = CARTESIAN_POINT ( 'NONE',  ( -7.685661446562381371, 5.583959896777970222, 4.006742014460233925 ) ) ;
#1090 = DIRECTION ( 'NONE',  ( 0.000000000000000000, 0.000000000000000000, 1.000000000000000000 ) ) ;
#1091 = VERTEX_POINT ( 'NONE', #11199 ) ;
#1092 = DIRECTION ( 'NONE',  ( 0.000000000000000000, -1.000000000000000000, 0.000000000000000000 ) ) ;
#1093 = DIRECTION ( 'NONE',  ( -1.000000000000000000, 0.000000000000000000, -0.000000000000000000 ) ) ;
#1094 = EDGE_LOOP ( 'NONE', ( #16293, #2195, #17387, #4639, #797 ) ) ;
#1095 = CARTESIAN_POINT ( 'NONE',  ( 0.000000000000000000, -6.393861490227931377, 9.782270569456429143 ) ) ;
#1096 = EDGE_LOOP ( 'NONE', ( #18272, #21824, #5313 ) ) ;
#1097 = CARTESIAN_POINT ( 'NONE',  ( 0.000000000000000000, 0.000000000000000000, 27.00000000000000000 ) ) ;
#1098 = DIRECTION ( 'NONE',  ( -0.000000000000000000, -0.000000000000000000, -1.000000000000000000 ) ) ;
#1099 = LINE ( 'NONE', #2672, #20811 ) ;
#1100 = ORIENTED_EDGE ( 'NONE', *, *, #17516, .T. ) ;
#1101 = EDGE_LOOP ( 'NONE', ( #10795, #24093, #23817, #6068 ) ) ;
#1102 = ORIENTED_EDGE ( 'NONE', *, *, #4855, .F. ) ;
#1103 = CARTESIAN_POINT ( 'NONE',  ( -9.499999999999790390, -3.086737114213257804, 7.159589141758144315 ) ) ;
#1104 = EDGE_CURVE ( 'NONE', #21150, #1494, #19983, .T. ) ;
#1105 = CARTESIAN_POINT ( 'NONE',  ( -7.685661446561619314, -5.583959896779019161, 12.40674201446023339 ) ) ;
#1106 = ADVANCED_FACE ( 'NONE', ( #13546 ), #11370, .T. ) ;
#1107 = AXIS2_PLACEMENT_3D ( 'NONE', #18511, #13000, #18268 ) ;
#1108 = ORIENTED_EDGE ( 'NONE', *, *, #14718, .T. ) ;
#1109 = DIRECTION ( 'NONE',  ( -4.625929269271481378E-15, 1.000000000000000000, -2.139922160430260066E-29 ) ) ;
#1110 = DIRECTION ( 'NONE',  ( -0.000000000000000000, -0.000000000000000000, 1.000000000000000000 ) ) ;
#1111 = DIRECTION ( 'NONE',  ( -0.5000000000000034417, 0.000000000000000000, 0.8660254037844367092 ) ) ;
#1112 = DIRECTION ( 'NONE',  ( -1.000000000000000000, -1.224606353822377258E-16, -0.000000000000000000 ) ) ;
#1113 = DIRECTION ( 'NONE',  ( -1.000000000000000000, -1.224606353822377258E-16, -0.000000000000000000 ) ) ;
#1114 = ORIENTED_EDGE ( 'NONE', *, *, #14057, .T. ) ;
#1115 = ORIENTED_EDGE ( 'NONE', *, *, #14350, .T. ) ;
#1116 = FACE_OUTER_BOUND ( 'NONE', #23887, .T. ) ;
#1117 = VERTEX_POINT ( 'NONE', #9366 ) ;
#1118 = DIRECTION ( 'NONE',  ( -1.000000000000000000, 0.000000000000000000, 0.000000000000000000 ) ) ;
#1119 = FILL_AREA_STYLE_COLOUR ( '', #2468 ) ;
#1120 = PRODUCT_RELATED_PRODUCT_CATEGORY ( 'part', '', ( #5703 ) ) ;
#1121 = DIRECTION ( 'NONE',  ( 0.000000000000000000, 0.000000000000000000, 1.000000000000000000 ) ) ;
#1122 = DIRECTION ( 'NONE',  ( -0.000000000000000000, -0.000000000000000000, -1.000000000000000000 ) ) ;
#1123 = EDGE_CURVE ( 'NONE', #19436, #145, #9058, .T. ) ;
#1124 = LINE ( 'NONE', #15987, #1184 ) ;
#1125 = ORIENTED_EDGE ( 'NONE', *, *, #20267, .F. ) ;
#1126 = DIRECTION ( 'NONE',  ( 0.000000000000000000, -1.000000000000000000, 0.000000000000000000 ) ) ;
#1127 = ADVANCED_FACE ( 'NONE', ( #9265 ), #23096, .F. ) ;
#1128 = ORIENTED_EDGE ( 'NONE', *, *, #11602, .F. ) ;
#1129 = CARTESIAN_POINT ( 'NONE',  ( 42.00000000000000000, -26.82133436441678853, 11.00000000000000000 ) ) ;
#1130 = ORIENTED_EDGE ( 'NONE', *, *, #18210, .F. ) ;
#1131 = CARTESIAN_POINT ( 'NONE',  ( 81.27272727272728048, 7.491529369508391930E-15, 0.000000000000000000 ) ) ;
#1132 = EDGE_CURVE ( 'NONE', #15963, #23778, #22705, .T. ) ;
#1133 = VECTOR ( 'NONE', #6566, 1000.000000000000000 ) ;
#1134 = EDGE_CURVE ( 'NONE', #15133, #11364, #17069, .T. ) ;
#1135 = DIRECTION ( 'NONE',  ( 1.000000000000000000, 0.000000000000000000, 0.000000000000000000 ) ) ;
#1136 = CARTESIAN_POINT ( 'NONE',  ( 60.32931906745326245, 7.420530141404717394E-15, 0.000000000000000000 ) ) ;
#1137 = DIRECTION ( 'NONE',  ( -0.000000000000000000, 0.000000000000000000, 1.000000000000000000 ) ) ;
#1138 = CARTESIAN_POINT ( 'NONE',  ( 65.85249911436491743, -5.000000000000000000, 6.123233995736775157E-16 ) ) ;
#1139 = VERTEX_POINT ( 'NONE', #19151 ) ;
#1140 = DIRECTION ( 'NONE',  ( 1.000000000000000000, 0.000000000000000000, -0.000000000000000000 ) ) ;
#1141 = CARTESIAN_POINT ( 'NONE',  ( 2.935661446562616295, -9.035036904803758873, -11.65958914175814520 ) ) ;
#1142 = EDGE_LOOP ( 'NONE', ( #5094, #17479, #5105, #5421, #6671 ) ) ;
#1143 = ORIENTED_EDGE ( 'NONE', *, *, #13907, .T. ) ;
#1144 = DIRECTION ( 'NONE',  ( 0.000000000000000000, -1.000000000000000000, 0.000000000000000000 ) ) ;
#1145 = CLOSED_SHELL ( 'NONE', ( #17694, #13029, #8993, #840, #11472, #14015, #20301, #5214, #16715, #7143, #23558, #13583, #21732, #537 ) ) ;
#1146 = CYLINDRICAL_SURFACE ( 'NONE', #21356, 8.000000000000000000 ) ;
#1147 = ORIENTED_EDGE ( 'NONE', *, *, #10934, .T. ) ;
#1148 = CARTESIAN_POINT ( 'NONE',  ( -2.000000000000000000, 0.000000000000000000, 6.000000000000000000 ) ) ;
#1149 = EDGE_CURVE ( 'NONE', #1494, #15963, #2317, .T. ) ;
#1150 = ORIENTED_EDGE ( 'NONE', *, *, #5309, .T. ) ;
#1151 = FACE_OUTER_BOUND ( 'NONE', #22912, .T. ) ;
#1152 = DIRECTION ( 'NONE',  ( 1.000000000000000000, 0.000000000000000000, 0.000000000000000000 ) ) ;
#1153 = CARTESIAN_POINT ( 'NONE',  ( -17.25000000000000000, 15.50000000000000000, 7.700000000000001954 ) ) ;
#1154 = CARTESIAN_POINT ( 'NONE',  ( -2.999999999999995559, 8.485281374238571317, 105.0000000000000000 ) ) ;
#1155 =( BOUNDED_CURVE ( )  B_SPLINE_CURVE ( 2, ( #3711, #7247, #12841, #7455, #3825, #9187, #11122, #16987, #5526, #11487, #5781 ),
 .UNSPECIFIED., .F., .T. ) 
 B_SPLINE_CURVE_WITH_KNOTS ( ( 3, 2, 2, 2, 2, 3 ),
 ( 0.3000000000000000999, 0.3200000000000001177, 0.3400000000000000799, 0.3600000000000000422, 0.3800000000000000044, 0.4000000000000000222 ),
 .UNSPECIFIED. ) 
 CURVE ( )  GEOMETRIC_REPRESENTATION_ITEM ( )  RATIONAL_B_SPLINE_CURVE ( ( 0.9999999999999997780, 0.9510565162951537532, 1.000000000000000000, 0.9510565162951535312, 1.000000000000000000, 0.9510565162951535312, 1.000000000000000000, 0.9510565162951535312, 1.000000000000000000, 0.9510565162951535312, 1.000000000000000000 ) ) 
 REPRESENTATION_ITEM ( '' )  );
#1156 = FACE_OUTER_BOUND ( 'NONE', #13713, .T. ) ;
#1157 = ORIENTED_EDGE ( 'NONE', *, *, #6133, .T. ) ;
#1158 = LINE ( 'NONE', #5408, #4856 ) ;
#1159 = DIRECTION ( 'NONE',  ( -1.000000000000000000, 0.000000000000000000, 0.000000000000000000 ) ) ;
#1160 = EDGE_CURVE ( 'NONE', #5396, #13970, #20, .T. ) ;
#1161 = LINE ( 'NONE', #10416, #16200 ) ;
#1162 = EDGE_CURVE ( 'NONE', #6139, #5924, #8274, .T. ) ;
#1163 = CARTESIAN_POINT ( 'NONE',  ( -2.935661446562617183, 9.035036904803758873, 6.659589141758144315 ) ) ;
#1164 = AXIS2_PLACEMENT_3D ( 'NONE', #9744, #17201, #7925 ) ;
#1165 = EDGE_LOOP ( 'NONE', ( #10490, #5286, #15472, #18274 ) ) ;
#1167 = ORIENTED_EDGE ( 'NONE', *, *, #22736, .F. ) ;
#1166 = CIRCLE ( 'NONE', #11647, 2.024999999999999911 ) ;
#1168 = ORIENTED_EDGE ( 'NONE', *, *, #1782, .F. ) ;
#1169 = ORIENTED_EDGE ( 'NONE', *, *, #3377, .T. ) ;
#1170 = LINE ( 'NONE', #6896, #17807 ) ;
#1171 = DIRECTION ( 'NONE',  ( 0.000000000000000000, 0.000000000000000000, 1.000000000000000000 ) ) ;
#1172 = DIRECTION ( 'NONE',  ( -0.000000000000000000, -0.000000000000000000, -1.000000000000000000 ) ) ;
#1173 = ORIENTED_EDGE ( 'NONE', *, *, #12448, .F. ) ;
#1174 = CARTESIAN_POINT ( 'NONE',  ( -17.05196227081077609, -8.053793831531462999, 5.044162359773902260 ) ) ;
#1175 = CARTESIAN_POINT ( 'NONE',  ( 40.66734255040738333, 26.56420859267091217, -3.000000000000000000 ) ) ;
#1176 = ORIENTED_EDGE ( 'NONE', *, *, #20506, .F. ) ;
#1177 = CARTESIAN_POINT ( 'NONE',  ( 23.00000000000000000, 0.000000000000000000, 0.000000000000000000 ) ) ;
#1178 = CARTESIAN_POINT ( 'NONE',  ( 63.23840997654417606, 7.420530141404717394E-15, 0.000000000000000000 ) ) ;
#1179 = PLANE ( 'NONE',  #515 ) ;
#1180 = DIRECTION ( 'NONE',  ( -0.000000000000000000, -0.000000000000000000, -1.000000000000000000 ) ) ;
#1181 = CARTESIAN_POINT ( 'NONE',  ( 5.871322893123448239, 8.081182679344781405, 4.359589141758143604 ) ) ;
#1182 = CIRCLE ( 'NONE', #9656, 1.999999999999994449 ) ;
#1183 = CARTESIAN_POINT ( 'NONE',  ( 16.36153765883234712, -6.593687918952693572, -6.842832175870683820 ) ) ;
#1184 = VECTOR ( 'NONE', #4549, 1000.000000000000000 ) ;
#1185 = DIRECTION ( 'NONE',  ( 0.000000000000000000, -1.000000000000000000, 0.000000000000000000 ) ) ;
#1186 = CYLINDRICAL_SURFACE ( 'NONE', #8299, 1.500000000000001332 ) ;
#1187 = ADVANCED_FACE ( 'NONE', ( #7670 ), #11312, .T. ) ;
#1188 = EDGE_CURVE ( 'NONE', #7839, #19249, #13280, .T. ) ;
#1189 = ORIENTED_EDGE ( 'NONE', *, *, #10741, .F. ) ;
#1190 = ORIENTED_EDGE ( 'NONE', *, *, #1629, .F. ) ;
#1191 = ORIENTED_EDGE ( 'NONE', *, *, #9608, .F. ) ;
#1192 = DIRECTION ( 'NONE',  ( -1.000000000000000000, 4.805184028455757624E-16, 8.408933298497764387E-17 ) ) ;
#1193 = DIRECTION ( 'NONE',  ( 0.000000000000000000, 0.000000000000000000, 1.000000000000000000 ) ) ;
#1194 = ORIENTED_EDGE ( 'NONE', *, *, #18665, .F. ) ;
#1195 = ORIENTED_EDGE ( 'NONE', *, *, #63, .T. ) ;
#1196 = DIRECTION ( 'NONE',  ( 0.000000000000000000, -1.000000000000000000, 0.000000000000000000 ) ) ;
#1197 = CARTESIAN_POINT ( 'NONE',  ( 7.685661446562381371, -5.583959896777971110, -7.859589141758143604 ) ) ;
#1198 = CIRCLE ( 'NONE', #3135, 20.85000000000000142 ) ;
#1199 = CARTESIAN_POINT ( 'NONE',  ( 0.3943934708257424981, 8.993434178613792795, 101.9804670325896012 ) ) ;
#1200 = CARTESIAN_POINT ( 'NONE',  ( -41.00000000000000000, 4.000000000000000888, 8.500000000000000000 ) ) ;
#1201 = CARTESIAN_POINT ( 'NONE',  ( -6.153822176767817416E-13, 9.500000000000000000, 3.568914004820076702 ) ) ;
#1202 = ADVANCED_FACE ( 'NONE', ( #19406 ), #1224, .F. ) ;
#1203 = ORIENTED_EDGE ( 'NONE', *, *, #9730, .F. ) ;
#1204 = DIRECTION ( 'NONE',  ( 0.000000000000000000, 1.000000000000000000, 0.000000000000000000 ) ) ;
#1205 = ADVANCED_FACE ( 'NONE', ( #12532 ), #8625, .T. ) ;
#1206 = DIRECTION ( 'NONE',  ( 0.000000000000000000, 0.000000000000000000, 1.000000000000000000 ) ) ;
#1207 = VERTEX_POINT ( 'NONE', #10711 ) ;
#1208 = DIRECTION ( 'NONE',  ( 0.000000000000000000, -1.000000000000000000, 0.000000000000000000 ) ) ;
#1209 = DIRECTION ( 'NONE',  ( 0.000000000000000000, -1.000000000000000000, 0.000000000000000000 ) ) ;
#1210 = CARTESIAN_POINT ( 'NONE',  ( 57.42022815836235594, 7.420530141404717394E-15, 0.000000000000000000 ) ) ;
#1211 = EDGE_CURVE ( 'NONE', #16656, #17382, #17580, .T. ) ;
#1212 = ADVANCED_FACE ( 'NONE', ( #14618 ), #14375, .F. ) ;
#1213 = FACE_OUTER_BOUND ( 'NONE', #5508, .T. ) ;
#1214 = ORIENTED_EDGE ( 'NONE', *, *, #7886, .T. ) ;
#1215 = CARTESIAN_POINT ( 'NONE',  ( 9.500000000000000000, 6.470877716354879437E-13, -13.20674201446023410 ) ) ;
#1216 = ORIENTED_EDGE ( 'NONE', *, *, #15855, .T. ) ;
#1217 = ORIENTED_EDGE ( 'NONE', *, *, #4231, .T. ) ;
#1218 = CIRCLE ( 'NONE', #14436, 17.87500000001787726 ) ;
#1219 = CARTESIAN_POINT ( 'NONE',  ( -7.685661446562381371, 5.583959896777970222, 2.859589141758144493 ) ) ;
#1220 = CARTESIAN_POINT ( 'NONE',  ( -9.500000000000000000, -6.482511860946779655E-13, 10.20674201446023233 ) ) ;
#1221 = DIRECTION ( 'NONE',  ( -1.000000000000000000, 0.000000000000000000, 0.000000000000000000 ) ) ;
#1222 = EDGE_LOOP ( 'NONE', ( #8792, #14858, #1855, #22422 ) ) ;
#1223 = DIRECTION ( 'NONE',  ( 1.000000000000000000, 0.000000000000000000, 0.000000000000000000 ) ) ;
#1224 = PLANE ( 'NONE',  #13343 ) ;
#1225 = LINE ( 'NONE', #11812, #16572 ) ;
#1226 = CARTESIAN_POINT ( 'NONE',  ( 7.685661446562381371, -5.583959896777971110, -5.006742014460233037 ) ) ;
#1227 = CARTESIAN_POINT ( 'NONE',  ( 28.27483331787887622, 41.23752903419610050, 27.00000000000000000 ) ) ;
#1228 = LINE ( 'NONE', #990, #5175 ) ;
#1229 = ADVANCED_FACE ( 'NONE', ( #1477 ), #18184, .T. ) ;
#1230 = CARTESIAN_POINT ( 'NONE',  ( 33.99999999999998579, 3.999999999999985345, 10.49999999999999822 ) ) ;
#1231 = VERTEX_POINT ( 'NONE', #23781 ) ;
#1232 = VECTOR ( 'NONE', #8932, 1000.000000000000000 ) ;
#1233 = EDGE_CURVE ( 'NONE', #19491, #18312, #7052, .T. ) ;
#1234 = DIRECTION ( 'NONE',  ( 0.000000000000000000, -1.000000000000000000, 0.000000000000000000 ) ) ;
#1235 = DIRECTION ( 'NONE',  ( 0.000000000000000000, -1.000000000000000000, 0.000000000000000000 ) ) ;
#1236 = VECTOR ( 'NONE', #332, 1000.000000000000000 ) ;
#1237 = CARTESIAN_POINT ( 'NONE',  ( 0.000000000000000000, 0.000000000000000000, 5.499999999999997335 ) ) ;
#1238 = DIRECTION ( 'NONE',  ( -1.000000000000000000, 0.000000000000000000, 0.000000000000000000 ) ) ;
#1239 = CARTESIAN_POINT ( 'NONE',  ( -42.00000000000000000, -4.000000000000000888, 10.49999999999999822 ) ) ;
#1240 = VERTEX_POINT ( 'NONE', #5239 ) ;
#1241 = DIRECTION ( 'NONE',  ( -0.000000000000000000, -0.000000000000000000, -1.000000000000000000 ) ) ;
#1242 = EDGE_LOOP ( 'NONE', ( #21780, #12311, #3570, #18097, #612 ) ) ;
#1243 = CARTESIAN_POINT ( 'NONE',  ( 5.871322893123448239, 8.081182679344781405, -6.359589141758142716 ) ) ;
#1244 = ORIENTED_EDGE ( 'NONE', *, *, #10076, .T. ) ;
#1245 = DIRECTION ( 'NONE',  ( -1.000000000000000000, -0.000000000000000000, -0.000000000000000000 ) ) ;
#1246 = VERTEX_POINT ( 'NONE', #12664 ) ;
#1247 = DIRECTION ( 'NONE',  ( 0.000000000000000000, 0.000000000000000000, 1.000000000000000000 ) ) ;
#1248 = DIRECTION ( 'NONE',  ( -0.000000000000000000, -0.000000000000000000, -1.000000000000000000 ) ) ;
#1249 = CIRCLE ( 'NONE', #17206, 5.000000000000007994 ) ;
#1250 = CARTESIAN_POINT ( 'NONE',  ( 70.21613547800127719, -1.078520768856852078E-29, 5.000000000000007994 ) ) ;
#1251 = CONICAL_SURFACE ( 'NONE', #6300, 5.000000000000007994, 0.9599310885968855844 ) ;
#1252 = DIRECTION ( 'NONE',  ( -1.000000000000000000, 0.000000000000000000, -0.000000000000000000 ) ) ;
#1253 = EDGE_CURVE ( 'NONE', #1785, #19039, #20133, .T. ) ;
#1254 = CARTESIAN_POINT ( 'NONE',  ( -5.871322893124554021, 8.081182679343978492, -5.906742014460233392 ) ) ;
#1255 = ORIENTED_EDGE ( 'NONE', *, *, #14400, .T. ) ;
#1256 = EDGE_LOOP ( 'NONE', ( #10196, #22504, #16988, #19893 ) ) ;
#1257 = CARTESIAN_POINT ( 'NONE',  ( -4.286858344475962035, -8.121112198674618199, -12.32511944772321044 ) ) ;
#1258 = ADVANCED_FACE ( 'NONE', ( #16086 ), #8994, .F. ) ;
#1259 = ADVANCED_FACE ( 'NONE', ( #14264 ), #22709, .T. ) ;
#1260 = LINE ( 'NONE', #16138, #4641 ) ;
#1261 = CIRCLE ( 'NONE', #18405, 0.2999999999999999334 ) ;
#1262 = VECTOR ( 'NONE', #20970, 1000.000000000000000 ) ;
#1263 = CONICAL_SURFACE ( 'NONE', #16052, 5.000000000000007994, 0.9599310885968855844 ) ;
#1264 = EDGE_LOOP ( 'NONE', ( #5368, #8367, #12828, #5738 ) ) ;
#1265 = PRODUCT_DEFINITION_SHAPE ( 'NONE', 'NONE',  #24101 ) ;
#1266 = CARTESIAN_POINT ( 'NONE',  ( 83.30704456891035647, 6.123233995736675563E-16, -5.000000000000007994 ) ) ;
#1267 = CIRCLE ( 'NONE', #19179, 5.000000000000007994 ) ;
#1268 = CYLINDRICAL_SURFACE ( 'NONE', #6767, 11.24716442891539714 ) ;
#1269 = DIRECTION ( 'NONE',  ( 0.000000000000000000, 0.000000000000000000, 1.000000000000000000 ) ) ;
#1270 = ORIENTED_EDGE ( 'NONE', *, *, #18092, .T. ) ;
#1271 = CARTESIAN_POINT ( 'NONE',  ( 7.685661446561619314, 5.583959896779020049, -9.406742014460235168 ) ) ;
#1272 = DIRECTION ( 'NONE',  ( -0.000000000000000000, -0.000000000000000000, -1.000000000000000000 ) ) ;
#1273 = DIRECTION ( 'NONE',  ( -0.000000000000000000, -0.000000000000000000, -1.000000000000000000 ) ) ;
#1274 = FACE_OUTER_BOUND ( 'NONE', #10623, .T. ) ;
#1275 = ORIENTED_EDGE ( 'NONE', *, *, #17876, .T. ) ;
#1276 = EDGE_CURVE ( 'NONE', #21393, #1240, #4758, .T. ) ;
#1277 = VECTOR ( 'NONE', #2666, 1000.000000000000000 ) ;
#1278 = ORIENTED_EDGE ( 'NONE', *, *, #108, .T. ) ;
#1279 = CIRCLE ( 'NONE', #6316, 9.499999999999994671 ) ;
#1281 = VECTOR ( 'NONE', #16204, 1000.000000000000000 ) ;
#1280 = PLANE ( 'NONE',  #22473 ) ;
#1282 = CONICAL_SURFACE ( 'NONE', #13742, 4.172000000000008590, 0.9599310885968742602 ) ;
#1283 = ADVANCED_FACE ( 'NONE', ( #17023 ), #13608, .T. ) ;
#1284 = DIRECTION ( 'NONE',  ( 0.000000000000000000, 0.000000000000000000, 1.000000000000000000 ) ) ;
#1285 = DIRECTION ( 'NONE',  ( -1.000000000000000000, -0.000000000000000000, -0.000000000000000000 ) ) ;
#1286 = DIRECTION ( 'NONE',  ( 0.000000000000000000, 0.000000000000000000, 1.000000000000000000 ) ) ;
#1287 = CIRCLE ( 'NONE', #10595, 0.9999999999999991118 ) ;
#1288 = EDGE_CURVE ( 'NONE', #7244, #1654, #19160, .T. ) ;
#1289 = EDGE_CURVE ( 'NONE', #14785, #19122, #19106, .T. ) ;
#1290 = CARTESIAN_POINT ( 'NONE',  ( 20.84999999999999432, -15.04000000000000448, -25.00000000000000000 ) ) ;
#1291 = VECTOR ( 'NONE', #14403, 1000.000000000000114 ) ;
#1292 = ORIENTED_EDGE ( 'NONE', *, *, #21074, .T. ) ;
#1293 = DIRECTION ( 'NONE',  ( -1.000000000000000000, -0.000000000000000000, -0.000000000000000000 ) ) ;
#1294 =( BOUNDED_CURVE ( )  B_SPLINE_CURVE ( 3, ( #3752, #12733, #3865, #7391 ),
 .UNSPECIFIED., .F., .T. ) 
 B_SPLINE_CURVE_WITH_KNOTS ( ( 4, 4 ),
 ( 3.141592653589793116, 4.712388980384689674 ),
 .UNSPECIFIED. ) 
 CURVE ( )  GEOMETRIC_REPRESENTATION_ITEM ( )  RATIONAL_B_SPLINE_CURVE ( ( 1.000000000000000000, 0.8047378541243649375, 0.8047378541243649375, 1.000000000000000000 ) ) 
 REPRESENTATION_ITEM ( '' )  );
#1295 = DIRECTION ( 'NONE',  ( -0.000000000000000000, -0.000000000000000000, -1.000000000000000000 ) ) ;
#1296 = CARTESIAN_POINT ( 'NONE',  ( -14.51962751333973856, 3.765689428759025681, 8.721787840009204373 ) ) ;
#1297 = CYLINDRICAL_SURFACE ( 'NONE', #8148, 14.99999999999999822 ) ;
#1298 = CARTESIAN_POINT ( 'NONE',  ( 0.000000000000000000, 2.342598717236902939, -4.057500000000001883 ) ) ;
#1299 = CARTESIAN_POINT ( 'NONE',  ( -14.79227890392045275, -2.568991289487079221, 9.169086800441911933 ) ) ;
#1301 = AXIS2_PLACEMENT_3D ( 'NONE', #9692, #13500, #20948 ) ;
#1300 = B_SPLINE_CURVE_WITH_KNOTS ( 'NONE', 3,
 ( #11944, #19410, #376, #13420, #21362, #2686, #15731, #4653 ),
 .UNSPECIFIED., .F., .F.,
 ( 4, 2, 2, 4 ),
 ( 0.003892319173193277415, 0.004864202078960305070, 0.005836084984727332725, 0.007779850796261388902 ),
 .UNSPECIFIED. ) ;
#1302 = DIRECTION ( 'NONE',  ( 1.000000000000000000, 0.000000000000000000, 0.000000000000000000 ) ) ;
#1303 = CARTESIAN_POINT ( 'NONE',  ( 0.000000000000000000, 15.03999999999999737, 0.000000000000000000 ) ) ;
#1304 = CIRCLE ( 'NONE', #18051, 2.024999999999999911 ) ;
#1305 = AXIS2_PLACEMENT_3D ( 'NONE', #12854, #11502, #22623 ) ;
#1306 = ORIENTED_EDGE ( 'NONE', *, *, #3440, .T. ) ;
#1307 = FACE_OUTER_BOUND ( 'NONE', #19962, .T. ) ;
#1308 = ORIENTED_EDGE ( 'NONE', *, *, #6819, .F. ) ;
#1309 = VECTOR ( 'NONE', #20266, 1000.000000000000000 ) ;
#1310 = CARTESIAN_POINT ( 'NONE',  ( -2.682529543899159208, -8.255977015246598327, 6.033165578109189298 ) ) ;
#1311 = VECTOR ( 'NONE', #15595, 1000.000000000000000 ) ;
#1312 = CARTESIAN_POINT ( 'NONE',  ( 693.7818939062880190, 888.4837211537981148, 1290.481724745928204 ) ) ;
#1313 = EDGE_CURVE ( 'NONE', #2368, #2794, #21051, .T. ) ;
#1314 = DIRECTION ( 'NONE',  ( 0.000000000000000000, 0.000000000000000000, 1.000000000000000000 ) ) ;
#1315 = VERTEX_POINT ( 'NONE', #13495 ) ;
#1316 = DIRECTION ( 'NONE',  ( -0.000000000000000000, -0.000000000000000000, 1.000000000000000000 ) ) ;
#1317 = CARTESIAN_POINT ( 'NONE',  ( -9.499999999999790390, -3.086737114213257804, -9.159589141758145203 ) ) ;
#1318 = CARTESIAN_POINT ( 'NONE',  ( -41.99999999999999289, 25.93535998569253920, 27.00000000000000000 ) ) ;
#1319 = CARTESIAN_POINT ( 'NONE',  ( -5.799656021750657521E-13, 8.953898637140671468, 3.324357723559535849 ) ) ;
#1320 = DIRECTION ( 'NONE',  ( -0.5579568342432784656, 0.8298699724181003434, 0.000000000000000000 ) ) ;
#1321 = EDGE_CURVE ( 'NONE', #13357, #18348, #16409, .T. ) ;
#1322 = VECTOR ( 'NONE', #1861, 1000.000000000000000 ) ;
#1323 = FACE_OUTER_BOUND ( 'NONE', #23964, .T. ) ;
#1324 = ORIENTED_EDGE ( 'NONE', *, *, #17103, .F. ) ;
#1325 = VECTOR ( 'NONE', #17373, 1000.000000000000000 ) ;
#1326 = FACE_OUTER_BOUND ( 'NONE', #12184, .T. ) ;
#1327 = AXIS2_PLACEMENT_3D ( 'NONE', #19592, #10160, #2869 ) ;
#1328 = CIRCLE ( 'NONE', #531, 4.249999999999996447 ) ;
#1329 = CIRCLE ( 'NONE', #212, 11.23082370883260417 ) ;
#1330 = DIRECTION ( 'NONE',  ( -1.000000000000000000, -1.224606353822377258E-16, -0.000000000000000000 ) ) ;
#1331 = ORIENTED_EDGE ( 'NONE', *, *, #22070, .F. ) ;
#1332 = CARTESIAN_POINT ( 'NONE',  ( -40.50000000000000711, 50.99999999999999289, 12.50000000000000000 ) ) ;
#1333 = CYLINDRICAL_SURFACE ( 'NONE', #18013, 5.000000000000000888 ) ;
#1334 = AXIS2_PLACEMENT_3D ( 'NONE', #16666, #14588, #19768 ) ;
#1335 = CARTESIAN_POINT ( 'NONE',  ( 29.00000000000000000, -29.50000000000000355, 11.00000000000000000 ) ) ;
#1336 = CARTESIAN_POINT ( 'NONE',  ( 17.52854577772373190, 9.313395544511452684, 1.935253206038901608 ) ) ;
#1337 = CARTESIAN_POINT ( 'NONE',  ( 23.00000000000000000, -7.812991839788663739, -16.07708877602020792 ) ) ;
#1338 = ORIENTED_EDGE ( 'NONE', *, *, #16996, .F. ) ;
#1339 = FACE_BOUND ( 'NONE', #4202, .T. ) ;
#1340 = CARTESIAN_POINT ( 'NONE',  ( -5.871322893124554021, 8.081182679343978492, -9.906742014460235168 ) ) ;
#1341 = FACE_OUTER_BOUND ( 'NONE', #185, .T. ) ;
#1342 = ORIENTED_EDGE ( 'NONE', *, *, #15135, .T. ) ;
#1343 = ORIENTED_EDGE ( 'NONE', *, *, #22854, .F. ) ;
#1344 = CARTESIAN_POINT ( 'NONE',  ( -2.935661446561384391, -9.035036904804158553, 12.60674201446023446 ) ) ;
#1345 = CARTESIAN_POINT ( 'NONE',  ( -7.685661446561619314, -5.583959896779019161, 4.406742014460233392 ) ) ;
#1346 = CIRCLE ( 'NONE', #8722, 5.025000000000002132 ) ;
#1347 = VERTEX_POINT ( 'NONE', #11889 ) ;
#1348 = AXIS2_PLACEMENT_3D ( 'NONE', #1136, #22346, #14763 ) ;
#1349 = DIRECTION ( 'NONE',  ( -1.000000000000000000, -0.000000000000000000, 0.000000000000000000 ) ) ;
#1350 = EDGE_CURVE ( 'NONE', #14353, #23778, #13360, .T. ) ;
#1351 = AXIS2_PLACEMENT_3D ( 'NONE', #14308, #23721, #4948 ) ;
#1352 = CARTESIAN_POINT ( 'NONE',  ( -5.871322893123449127, -8.081182679344781405, 3.359589141758143160 ) ) ;
#1353 = DIRECTION ( 'NONE',  ( 0.000000000000000000, 1.000000000000000000, 0.000000000000000000 ) ) ;
#1354 = CIRCLE ( 'NONE', #15750, 1.000000000000000888 ) ;
#1355 = AXIS2_PLACEMENT_3D ( 'NONE', #3508, #12518, #19991 ) ;
#1356 =( NAMED_UNIT ( * ) PLANE_ANGLE_UNIT ( ) SI_UNIT ( $, .RADIAN. ) );
#1357 = ADVANCED_FACE ( 'NONE', ( #17138 ), #6421, .F. ) ;
#1358 = DIRECTION ( 'NONE',  ( -1.000000000000000000, 0.000000000000000000, 0.000000000000000000 ) ) ;
#1359 = EDGE_CURVE ( 'NONE', #1240, #18394, #11389, .T. ) ;
#1360 = ORIENTED_EDGE ( 'NONE', *, *, #6186, .F. ) ;
#1361 = ORIENTED_EDGE ( 'NONE', *, *, #5824, .F. ) ;
#1362 = CARTESIAN_POINT ( 'NONE',  ( -34.00000000000000000, 4.999999999999999112, 10.49999999999999822 ) ) ;
#1363 = FACE_OUTER_BOUND ( 'NONE', #13402, .T. ) ;
#1364 = LINE ( 'NONE', #20019, #16835 ) ;
#1365 = SURFACE_STYLE_FILL_AREA ( #2948 ) ;
#1366 = VECTOR ( 'NONE', #20697, 1000.000000000000000 ) ;
#1367 = VECTOR ( 'NONE', #191, 1000.000000000000000 ) ;
#1368 = CARTESIAN_POINT ( 'NONE',  ( -42.00000000000000000, 6.000000000000000888, 10.49999999999999822 ) ) ;
#1369 = CARTESIAN_POINT ( 'NONE',  ( 8.680847955710813579, 2.820578480814259326, -8.733165578109185034 ) ) ;
#1370 = AXIS2_PLACEMENT_3D ( 'NONE', #19005, #447, #335 ) ;
#1371 = CARTESIAN_POINT ( 'NONE',  ( -14.51962751333973856, 3.765689428759025681, 8.721787840009204373 ) ) ;
#1372 = VERTEX_POINT ( 'NONE', #23138 ) ;
#1373 = DIRECTION ( 'NONE',  ( 0.000000000000000000, 0.4999999999999989453, -0.8660254037844392627 ) ) ;
#1374 = CIRCLE ( 'NONE', #575, 5.000000000000007994 ) ;
#1375 = ORIENTED_EDGE ( 'NONE', *, *, #3223, .T. ) ;
#1376 = LINE ( 'NONE', #5131, #16076 ) ;
#1377 = EDGE_CURVE ( 'NONE', #2165, #12612, #12118, .T. ) ;
#1378 = ORIENTED_EDGE ( 'NONE', *, *, #23194, .F. ) ;
#1379 = CARTESIAN_POINT ( 'NONE',  ( 23.00000000000000000, -2.110835303355205639, -14.05523051341068097 ) ) ;
#1380 = VECTOR ( 'NONE', #14711, 1000.000000000000000 ) ;
#1381 = CARTESIAN_POINT ( 'NONE',  ( -7.685661446561619314, -5.583959896779019161, -3.259589141758143516 ) ) ;
#1382 = ADVANCED_FACE ( 'NONE', ( #2145 ), #9572, .T. ) ;
#1383 = DIRECTION ( 'NONE',  ( 1.000000000000000000, 0.000000000000000000, 0.000000000000000000 ) ) ;
#1384 = VECTOR ( 'NONE', #10284, 1000.000000000000000 ) ;
#1385 = EDGE_LOOP ( 'NONE', ( #16104, #7716, #9103, #16213 ) ) ;
#1386 = DIRECTION ( 'NONE',  ( 1.000000000000000000, 0.000000000000000000, 0.000000000000000000 ) ) ;
#1387 = DIRECTION ( 'NONE',  ( -0.7071067811865660024, 8.659560562355159656E-17, 0.7071067811865291430 ) ) ;
#1388 = AXIS2_PLACEMENT_3D ( 'NONE', #6789, #3121, #23980 ) ;
#1389 = CARTESIAN_POINT ( 'NONE',  ( -7.685661446561619314, -5.583959896779019161, -6.406742014460233392 ) ) ;
#1390 = EDGE_LOOP ( 'NONE', ( #23022, #7636, #6946, #12939 ) ) ;
#1391 = CIRCLE ( 'NONE', #21637, 8.000000000000000000 ) ;
#1392 = FACE_OUTER_BOUND ( 'NONE', #706, .T. ) ;
#1393 = CYLINDRICAL_SURFACE ( 'NONE', #2791, 18.50000000000000000 ) ;
#1394 = CARTESIAN_POINT ( 'NONE',  ( 0.000000000000000000, 8.890849273385706297, -7.584660931657394300 ) ) ;
#1395 = CARTESIAN_POINT ( 'NONE',  ( 2.570122167802765922, 0.000000000000000000, 11.22592346138681130 ) ) ;
#1396 = AXIS2_PLACEMENT_3D ( 'NONE', #10949, #23697, #22335 ) ;
#1397 = CIRCLE ( 'NONE', #15795, 2.024999999999999911 ) ;
#1398 = EDGE_LOOP ( 'NONE', ( #20476, #23765, #11876, #1150, #21778 ) ) ;
#1399 = DIRECTION ( 'NONE',  ( -1.000000000000000000, 0.000000000000000000, 0.000000000000000000 ) ) ;
#1400 = DIRECTION ( 'NONE',  ( -1.000000000000000000, 0.000000000000000000, 0.000000000000000000 ) ) ;
#1401 = CARTESIAN_POINT ( 'NONE',  ( 27.99999999999998934, -51.00000000000000711, 0.5000000000000000000 ) ) ;
#1402 = EDGE_LOOP ( 'NONE', ( #19618, #10972, #14817, #21504 ) ) ;
#1403 =( REPRESENTATION_RELATIONSHIP ('NONE','NONE', #21748, #7043 ) REPRESENTATION_RELATIONSHIP_WITH_TRANSFORMATION ( #3932 )SHAPE_REPRESENTATION_RELATIONSHIP( ) );
#1404 = CARTESIAN_POINT ( 'NONE',  ( -45.00000000000001421, 50.99999999999992184, 12.50000000000000000 ) ) ;
#1405 = LINE ( 'NONE', #6890, #2438 ) ;
#1406 = LINE ( 'NONE', #3214, #23638 ) ;
#1407 = CARTESIAN_POINT ( 'NONE',  ( -9.499999999999790390, -3.086737114213257804, 3.159589141758143871 ) ) ;
#1408 = AXIS2_PLACEMENT_3D ( 'NONE', #7426, #374, #9266 ) ;
#1409 = VERTEX_POINT ( 'NONE', #15169 ) ;
#1410 = ADVANCED_FACE ( 'NONE', ( #22640 ), #5922, .F. ) ;
#1411 = EDGE_CURVE ( 'NONE', #11194, #10631, #9687, .T. ) ;
#1412 = AXIS2_PLACEMENT_3D ( 'NONE', #17511, #10058, #4724 ) ;
#1413 = VERTEX_POINT ( 'NONE', #8838 ) ;
#1414 = AXIS2_PLACEMENT_3D ( 'NONE', #10150, #13966, #15912 ) ;
#1415 = ORIENTED_EDGE ( 'NONE', *, *, #4785, .T. ) ;
#1416 = ORIENTED_EDGE ( 'NONE', *, *, #2608, .T. ) ;
#1417 = CARTESIAN_POINT ( 'NONE',  ( 65.27272727272728048, -4.172000000000000597, 0.000000000000000000 ) ) ;
#1418 = DIRECTION ( 'NONE',  ( 0.000000000000000000, 0.000000000000000000, 1.000000000000000000 ) ) ;
#1419 = CARTESIAN_POINT ( 'NONE',  ( -40.23082370883257397, -29.50000000000000711, -3.000000000000000000 ) ) ;
#1420 = ORIENTED_EDGE ( 'NONE', *, *, #14208, .T. ) ;
#1421 = EDGE_LOOP ( 'NONE', ( #21332, #19212, #5231, #17861 ) ) ;
#1422 = CIRCLE ( 'NONE', #6088, 5.000000000000007994 ) ;
#1423 = FACE_OUTER_BOUND ( 'NONE', #6483, .T. ) ;
#1424 = ORIENTED_EDGE ( 'NONE', *, *, #3648, .T. ) ;
#1425 = CYLINDRICAL_SURFACE ( 'NONE', #2968, 1.499999999999998002 ) ;
#1426 = LINE ( 'NONE', #18686, #16854 ) ;
#1428 = DIRECTION ( 'NONE',  ( -0.000000000000000000, -0.000000000000000000, -1.000000000000000000 ) ) ;
#1427 = CONICAL_SURFACE ( 'NONE', #23633, 4.172000000000008590, 0.9599310885968742602 ) ;
#1429 = CARTESIAN_POINT ( 'NONE',  ( 34.02500000000000568, -29.50000000000000000, -3.000000000000000000 ) ) ;
#1430 = DIRECTION ( 'NONE',  ( -1.000000000000000000, 0.000000000000000000, 0.000000000000000000 ) ) ;
#1431 = PRODUCT_DEFINITION ( 'UNKNOWN', '', #16228, #4583 ) ;
#1432 = VECTOR ( 'NONE', #18179, 1000.000000000000114 ) ;
#1433 = CARTESIAN_POINT ( 'NONE',  ( 14.51962751333974211, -3.765689428759034563, 8.721787840009190163 ) ) ;
#1434 = VECTOR ( 'NONE', #8639, 1000.000000000000000 ) ;
#1435 = ADVANCED_FACE ( 'NONE', ( #6656 ), #10166, .T. ) ;
#1436 = DIRECTION ( 'NONE',  ( -0.000000000000000000, 0.000000000000000000, 1.000000000000000000 ) ) ;
#1437 = CARTESIAN_POINT ( 'NONE',  ( -2.682529543899159208, -8.255977015246598327, -4.033165578109189298 ) ) ;
#1438 = ADVANCED_FACE ( 'NONE', ( #19945 ), #19840, .F. ) ;
#1439 = EDGE_LOOP ( 'NONE', ( #2545, #8145, #17255, #10137 ) ) ;
#1440 = CARTESIAN_POINT ( 'NONE',  ( 2.682529543899157876, 8.255977015246598327, 9.033165578109187521 ) ) ;
#1441 = ORIENTED_EDGE ( 'NONE', *, *, #11534, .T. ) ;
#1442 = ADVANCED_FACE ( 'NONE', ( #13204 ), #455, .F. ) ;
#1443 = EDGE_CURVE ( 'NONE', #2102, #12778, #15399, .T. ) ;
#1444 = SHAPE_DEFINITION_REPRESENTATION ( #8854, #1013 ) ;
#1445 =( GEOMETRIC_REPRESENTATION_CONTEXT ( 3 ) GLOBAL_UNCERTAINTY_ASSIGNED_CONTEXT ( ( #20850 ) ) GLOBAL_UNIT_ASSIGNED_CONTEXT ( ( #19253, #21330, #6565 ) ) REPRESENTATION_CONTEXT ( 'NONE', 'WORKASPACE' ) );
#1446 = DIRECTION ( 'NONE',  ( 1.000000000000000000, 0.000000000000000000, 0.000000000000000000 ) ) ;
#1447 = EDGE_LOOP ( 'NONE', ( #10380, #22647, #5919, #8431 ) ) ;
#1448 = EDGE_LOOP ( 'NONE', ( #8557, #14312, #18773, #7041 ) ) ;
#1449 = DIRECTION ( 'NONE',  ( -0.000000000000000000, -0.000000000000000000, -1.000000000000000000 ) ) ;
#1450 = CARTESIAN_POINT ( 'NONE',  ( 5.871322893124553133, -8.081182679343980269, -7.759589141758143072 ) ) ;
#1451 = AXIS2_PLACEMENT_3D ( 'NONE', #5361, #5014, #1694 ) ;
#1452 =( BOUNDED_SURFACE ( )  B_SPLINE_SURFACE ( 1, 2, ( 
 ( #9852, #8268, #19403, #4763, #6331, #13654, #22943, #20985, #1105, #6099, #2563, #10095, #2926, #21355, #21091, #4391, #9976, #23185, #4274, #12046, #19518, #2797, #17435, #17679, #10353, #10218, #734, #8406, #23316, #17816, #1220, #23429, #6948, #14479, #10472, #20128, #19775, #5109, #8631, #1573, #16084, #12780, #12660, #3404, #10820, #10706, #18178, #18289, #8769, #8987, #3279, #14370, #22082, #1472, #16432, #17932, #21827, #15968, #14258, #23546, #12421, #7175, #5355, #21949, #8885, #6828, #21720, #16217, #23897, #19882, #14612, #23777, #12528, #5007, #7049, #6704, #20240, #12305, #16322, #3517, #3158, #5233, #10925, #18397, #8526, #20000, #3050, #14136, #1345, #10582, #4893, #340, #9459, #20350, #13882, #13997, #13625 ),
 ( #4731, #19010, #22914, #15562, #17644, #17520, #9819, #15319, #20959, #2651, #2284, #6299, #2530, #11775, #4243, #4617, #10185, #11905, #22789, #6071, #19251, #15824, #11652, #9702, #17413, #821, #19121, #12018, #13512, #23024, #17282, #19490, #582, #23288, #2765, #949, #8372, #21196, #4501, #6563, #708, #21441, #10067, #8117, #17155, #8232, #6191, #21065, #15687, #4361, #8602, #3023, #16051, #11113, #9288, #1751, #12833, #21565, #12274, #3128, #10550, #2896, #16733, #7237, #20291, #18463, #1310, #23516, #10443, #20406, #19743, #6797, #3697, #5520, #14226, #4981, #7343, #8498, #9179, #39, #21686, #8734, #10323, #12392, #15941, #16186, #1079, #23646, #14677, #18594, #14901, #22140, #5411, #3566, #16628, #22247, #17783 ) ),
 .UNSPECIFIED., .F., .F., .T. ) 
 B_SPLINE_SURFACE_WITH_KNOTS ( ( 2, 2 ),
 ( 3, 2, 2, 2, 2, 2, 2, 2, 2, 2, 2, 2, 2, 2, 2, 2, 2, 2, 2, 2, 2, 2, 2, 2, 2, 2, 2, 2, 2, 2, 2, 2, 2, 2, 2, 2, 2, 2, 2, 2, 2, 2, 2, 2, 2, 2, 2, 2, 3 ),
 ( 0.000000000000000000, 1.000000000000000000 ),
 ( 0.000000000000000000, 0.02000000000000000042, 0.04000000000000000083, 0.05999999999999999778, 0.08000000000000000167, 0.1000000000000000056, 0.1199999999999999956, 0.1400000000000000133, 0.1600000000000000033, 0.1799999999999999933, 0.2000000000000000111, 0.2200000000000000011, 0.2399999999999999911, 0.2600000000000000089, 0.2800000000000000266, 0.2999999999999999889, 0.3200000000000000067, 0.3400000000000000244, 0.3599999999999999867, 0.3800000000000000044, 0.4000000000000000222, 0.4199999999999999845, 0.4400000000000000022, 0.4600000000000000200, 0.4799999999999999822, 0.5000000000000000000, 0.5200000000000000178, 0.5400000000000000355, 0.5600000000000000533, 0.5799999999999999600, 0.5999999999999999778, 0.6199999999999999956, 0.6400000000000000133, 0.6600000000000000311, 0.6800000000000000488, 0.6999999999999999556, 0.7199999999999999734, 0.7399999999999999911, 0.7600000000000000089, 0.7800000000000000266, 0.8000000000000000444, 0.8199999999999999512, 0.8399999999999999689, 0.8599999999999999867, 0.8800000000000000044, 0.9000000000000000222, 0.9200000000000000400, 0.9399999999999999467, 0.9500000000000000666 ),
 .UNSPECIFIED. ) 
 GEOMETRIC_REPRESENTATION_ITEM ( )  RATIONAL_B_SPLINE_SURFACE ( (
 ( 1.000000000000000000, 0.9510565162951535312, 1.000000000000000000, 0.9510565162951535312, 1.000000000000000000, 0.9510565162951535312, 1.000000000000000000, 0.9510565162951535312, 1.000000000000000000, 0.9510565162951535312, 1.000000000000000000, 0.9510565162951535312, 1.000000000000000000, 0.9510565162951535312, 1.000000000000000000, 0.9510565162951535312, 1.000000000000000000, 0.9510565162951535312, 1.000000000000000000, 0.9510565162951535312, 1.000000000000000000, 0.9510565162951535312, 1.000000000000000000, 0.9510565162951535312, 1.000000000000000000, 0.9510565162951535312, 1.000000000000000000, 0.9510565162951535312, 1.000000000000000000, 0.9510565162951535312, 1.000000000000000000, 0.9510565162951535312, 1.000000000000000000, 0.9510565162951535312, 1.000000000000000000, 0.9510565162951535312, 1.000000000000000000, 0.9510565162951535312, 1.000000000000000000, 0.9510565162951535312, 1.000000000000000000, 0.9510565162951535312, 1.000000000000000000, 0.9510565162951535312, 1.000000000000000000, 0.9510565162951535312, 1.000000000000000000, 0.9510565162951535312, 1.000000000000000000, 0.9510565162951535312, 1.000000000000000000, 0.9510565162951535312, 1.000000000000000000, 0.9510565162951535312, 1.000000000000000000, 0.9510565162951535312, 1.000000000000000000, 0.9510565162951535312, 1.000000000000000000, 0.9510565162951535312, 1.000000000000000000, 0.9510565162951535312, 1.000000000000000000, 0.9510565162951535312, 1.000000000000000000, 0.9510565162951535312, 1.000000000000000000, 0.9510565162951535312, 1.000000000000000000, 0.9510565162951535312, 1.000000000000000000, 0.9510565162951535312, 1.000000000000000000, 0.9510565162951535312, 1.000000000000000000, 0.9510565162951535312, 1.000000000000000000, 0.9510565162951535312, 1.000000000000000000, 0.9510565162951535312, 1.000000000000000000, 0.9510565162951535312, 1.000000000000000000, 0.9510565162951535312, 1.000000000000000000, 0.9510565162951535312, 1.000000000000000000, 0.9510565162951535312, 1.000000000000000000, 0.9510565162951535312, 1.000000000000000000, 0.9510565162951535312, 1.000000000000000000, 0.9510565162951535312, 1.000000000000000000, 0.9755282581475764880, 0.9755282581475768211),
 ( 1.000000000000000000, 0.9510565162951535312, 1.000000000000000000, 0.9510565162951535312, 1.000000000000000000, 0.9510565162951535312, 1.000000000000000000, 0.9510565162951535312, 1.000000000000000000, 0.9510565162951535312, 1.000000000000000000, 0.9510565162951535312, 1.000000000000000000, 0.9510565162951535312, 1.000000000000000000, 0.9510565162951535312, 1.000000000000000000, 0.9510565162951535312, 1.000000000000000000, 0.9510565162951535312, 1.000000000000000000, 0.9510565162951535312, 1.000000000000000000, 0.9510565162951535312, 1.000000000000000000, 0.9510565162951535312, 1.000000000000000000, 0.9510565162951535312, 1.000000000000000000, 0.9510565162951535312, 1.000000000000000000, 0.9510565162951535312, 1.000000000000000000, 0.9510565162951535312, 1.000000000000000000, 0.9510565162951535312, 1.000000000000000000, 0.9510565162951535312, 1.000000000000000000, 0.9510565162951535312, 1.000000000000000000, 0.9510565162951535312, 1.000000000000000000, 0.9510565162951535312, 1.000000000000000000, 0.9510565162951535312, 1.000000000000000000, 0.9510565162951535312, 1.000000000000000000, 0.9510565162951535312, 1.000000000000000000, 0.9510565162951535312, 1.000000000000000000, 0.9510565162951535312, 1.000000000000000000, 0.9510565162951535312, 1.000000000000000000, 0.9510565162951535312, 1.000000000000000000, 0.9510565162951535312, 1.000000000000000000, 0.9510565162951535312, 1.000000000000000000, 0.9510565162951535312, 1.000000000000000000, 0.9510565162951535312, 1.000000000000000000, 0.9510565162951535312, 1.000000000000000000, 0.9510565162951535312, 1.000000000000000000, 0.9510565162951535312, 1.000000000000000000, 0.9510565162951535312, 1.000000000000000000, 0.9510565162951535312, 1.000000000000000000, 0.9510565162951535312, 1.000000000000000000, 0.9510565162951535312, 1.000000000000000000, 0.9510565162951535312, 1.000000000000000000, 0.9510565162951535312, 1.000000000000000000, 0.9510565162951535312, 1.000000000000000000, 0.9510565162951535312, 1.000000000000000000, 0.9510565162951535312, 1.000000000000000000, 0.9510565162951535312, 1.000000000000000000, 0.9510565162951535312, 1.000000000000000000, 0.9755282581475764880, 0.9755282581475768211) ) ) 
 REPRESENTATION_ITEM ( '' )  SURFACE ( )  );
#1453 = DIRECTION ( 'NONE',  ( -0.000000000000000000, -0.000000000000000000, -1.000000000000000000 ) ) ;
#1454 = CARTESIAN_POINT ( 'NONE',  ( 78.94340820527399671, 5.000000000000015099, 0.000000000000000000 ) ) ;
#1455 = LINE ( 'NONE', #8863, #2548 ) ;
#1456 = CYLINDRICAL_SURFACE ( 'NONE', #4397, 23.85000000000000142 ) ;
#1457 = ORIENTED_EDGE ( 'NONE', *, *, #8924, .F. ) ;
#1458 = AXIS2_PLACEMENT_3D ( 'NONE', #3926, #9389, #167 ) ;
#1459 = LINE ( 'NONE', #5095, #23854 ) ;
#1460 = ORIENTED_EDGE ( 'NONE', *, *, #108, .F. ) ;
#1461 = DIRECTION ( 'NONE',  ( 1.000000000000000000, 0.000000000000000000, 0.000000000000000000 ) ) ;
#1462 = CYLINDRICAL_SURFACE ( 'NONE', #4833, 1.499999999999994449 ) ;
#1463 = CARTESIAN_POINT ( 'NONE',  ( 17.05196227081078320, 8.053793831531466552, 5.044162359773899595 ) ) ;
#1464 = EDGE_CURVE ( 'NONE', #14261, #22901, #12181, .T. ) ;
#1465 = LINE ( 'NONE', #14362, #15335 ) ;
#1466 = ORIENTED_EDGE ( 'NONE', *, *, #15552, .F. ) ;
#1467 = CARTESIAN_POINT ( 'NONE',  ( 0.000000000000000000, 0.000000000000000000, 0.000000000000000000 ) ) ;
#1468 = DIRECTION ( 'NONE',  ( -1.000000000000000000, -0.000000000000000000, 0.000000000000000000 ) ) ;
#1469 = VERTEX_POINT ( 'NONE', #5637 ) ;
#1470 = VERTEX_POINT ( 'NONE', #24055 ) ;
#1471 = CARTESIAN_POINT ( 'NONE',  ( -2.935661446561384391, -9.035036904804158553, 10.60674201446023446 ) ) ;
#1472 = CARTESIAN_POINT ( 'NONE',  ( -5.871322893124554021, 8.081182679343978492, 7.906742014460233392 ) ) ;
#1473 = EDGE_CURVE ( 'NONE', #16008, #4837, #510, .T. ) ;
#1474 = ORIENTED_EDGE ( 'NONE', *, *, #8163, .T. ) ;
#1475 = ADVANCED_FACE ( 'NONE', ( #20279 ), #1393, .F. ) ;
#1476 = ORIENTED_EDGE ( 'NONE', *, *, #20075, .T. ) ;
#1477 = FACE_OUTER_BOUND ( 'NONE', #14795, .T. ) ;
#1478 = CARTESIAN_POINT ( 'NONE',  ( -36.00000000000001421, 50.99999999999999289, 0.5000000000000004441 ) ) ;
#1479 = CARTESIAN_POINT ( 'NONE',  ( -9.500000000000211386, 3.086737114211961064, 2.959589141758143249 ) ) ;
#1480 = FACE_OUTER_BOUND ( 'NONE', #23076, .T. ) ;
#1481 = CARTESIAN_POINT ( 'NONE',  ( 66.72727272727273373, 7.491529369508391930E-15, 0.000000000000000000 ) ) ;
#1482 = FACE_OUTER_BOUND ( 'NONE', #16685, .T. ) ;
#1483 = FACE_OUTER_BOUND ( 'NONE', #13624, .T. ) ;
#1484 = EDGE_LOOP ( 'NONE', ( #8065, #13351, #5397, #1190 ) ) ;
#1485 = VERTEX_POINT ( 'NONE', #3449 ) ;
#1486 = DIRECTION ( 'NONE',  ( -1.000000000000000000, 0.000000000000000000, 0.000000000000000000 ) ) ;
#1487 = DIRECTION ( 'NONE',  ( -1.000000000000000000, -1.224606353822377258E-16, -0.000000000000000000 ) ) ;
#1488 = CARTESIAN_POINT ( 'NONE',  ( -3.053836969424609471, 9.001008217452133309, -3.499964733571762299 ) ) ;
#1489 = CARTESIAN_POINT ( 'NONE',  ( 0.000000000000000000, 0.000000000000000000, 15.50000000000000000 ) ) ;
#1490 = DIRECTION ( 'NONE',  ( 0.000000000000000000, -1.000000000000000000, 0.000000000000000000 ) ) ;
#1491 = ORIENTED_EDGE ( 'NONE', *, *, #4596, .T. ) ;
#1492 = CARTESIAN_POINT ( 'NONE',  ( -5.365059087799947335, 7.384370330706355290, -9.333165578109190008 ) ) ;
#1493 = DIRECTION ( 'NONE',  ( 1.000000000000000000, 0.000000000000000000, 0.000000000000000000 ) ) ;
#1494 = VERTEX_POINT ( 'NONE', #3553 ) ;
#1495 = CARTESIAN_POINT ( 'NONE',  ( -30.68762588338046982, -45.64284848299540442, -1.500000000000000000 ) ) ;
#1496 = ORIENTED_EDGE ( 'NONE', *, *, #15252, .F. ) ;
#1497 = CARTESIAN_POINT ( 'NONE',  ( 7.022953521755574080, -5.102474405759714671, 4.433165578109187877 ) ) ;
#1498 = EDGE_CURVE ( 'NONE', #1766, #13946, #15222, .T. ) ;
#1499 = ORIENTED_EDGE ( 'NONE', *, *, #11874, .T. ) ;
#1500 = CARTESIAN_POINT ( 'NONE',  ( -2.935661446562617183, 9.035036904803758873, -2.659589141758143871 ) ) ;
#1501 = DIRECTION ( 'NONE',  ( 1.000000000000000000, 0.000000000000000000, 0.000000000000000000 ) ) ;
#1502 = ORIENTED_EDGE ( 'NONE', *, *, #12364, .T. ) ;
#1503 = DIRECTION ( 'NONE',  ( -1.000000000000000000, -0.000000000000000000, -0.000000000000000000 ) ) ;
#1504 = CARTESIAN_POINT ( 'NONE',  ( 21.85000000000000497, 16.67999999999999972, 13.00000000000000178 ) ) ;
#1505 = AXIS2_PLACEMENT_3D ( 'NONE', #16896, #1795, #86 ) ;
#1506 = CARTESIAN_POINT ( 'NONE',  ( 6.809999908187194197E-13, -9.988891130263535700, -11.55958914175814201 ) ) ;
#1507 = VERTEX_POINT ( 'NONE', #14773 ) ;
#1508 = CARTESIAN_POINT ( 'NONE',  ( -6.153822176767817416E-13, 9.500000000000000000, -3.637828009640159621 ) ) ;
#1509 = FACE_OUTER_BOUND ( 'NONE', #11228, .T. ) ;
#1510 = EDGE_CURVE ( 'NONE', #22463, #3733, #23458, .T. ) ;
#1511 = ADVANCED_FACE ( 'NONE', ( #1509 ), #14411, .F. ) ;
#1512 = ORIENTED_EDGE ( 'NONE', *, *, #21726, .F. ) ;
#1513 = CARTESIAN_POINT ( 'NONE',  ( -27.89784171216405895, 41.49349862090491570, -3.000000000000000000 ) ) ;
#1514 = ORIENTED_EDGE ( 'NONE', *, *, #17, .F. ) ;
#1515 = CARTESIAN_POINT ( 'NONE',  ( 30.44534269664590909, -40.40463133211080304, 27.00000000000000000 ) ) ;
#1516 = EDGE_CURVE ( 'NONE', #2260, #13127, #5517, .T. ) ;
#1517 = CARTESIAN_POINT ( 'NONE',  ( 0.000000000000000000, -12.99147757894464306, 7.750000000000000000 ) ) ;
#1518 = CARTESIAN_POINT ( 'NONE',  ( 41.99999999999999289, 5.618459588085056979E-15, -10.50249999999999950 ) ) ;
#1519 = FACE_OUTER_BOUND ( 'NONE', #6255, .T. ) ;
#1520 = CIRCLE ( 'NONE', #7329, 6.500000000000000888 ) ;
#1521 = ORIENTED_EDGE ( 'NONE', *, *, #23487, .T. ) ;
#1522 = ORIENTED_EDGE ( 'NONE', *, *, #21971, .T. ) ;
#1523 = VERTEX_POINT ( 'NONE', #10860 ) ;
#1524 = ORIENTED_EDGE ( 'NONE', *, *, #18346, .F. ) ;
#1525 = DIRECTION ( 'NONE',  ( -0.000000000000000000, -0.000000000000000000, 1.000000000000000000 ) ) ;
#1526 = DIRECTION ( 'NONE',  ( -0.000000000000000000, 0.000000000000000000, 1.000000000000000000 ) ) ;
#1527 = ORIENTED_EDGE ( 'NONE', *, *, #4652, .T. ) ;
#1528 = ORIENTED_EDGE ( 'NONE', *, *, #15175, .T. ) ;
#1529 = CARTESIAN_POINT ( 'NONE',  ( -15.07341617659254318, -4.495283618570418582, -8.379779594489216166 ) ) ;
#1530 = CARTESIAN_POINT ( 'NONE',  ( -30.68762588338046982, -45.64284848299540442, 0.000000000000000000 ) ) ;
#1531 = VERTEX_POINT ( 'NONE', #16611 ) ;
#1532 = DIRECTION ( 'NONE',  ( -0.000000000000000000, -0.000000000000000000, -1.000000000000000000 ) ) ;
#1533 = CARTESIAN_POINT ( 'NONE',  ( -9.500000000000000000, -6.482511860946779655E-13, 6.206742014460234103 ) ) ;
#1534 = CYLINDRICAL_SURFACE ( 'NONE', #19218, 18.50000000000000000 ) ;
#1535 = ADVANCED_FACE ( 'NONE', ( #10751 ), #16033, .F. ) ;
#1536 = EDGE_CURVE ( 'NONE', #13092, #7965, #20749, .T. ) ;
#1537 = CARTESIAN_POINT ( 'NONE',  ( 5.000000000000000000, 4.685197434473818312, -1.301042606982605321E-15 ) ) ;
#1538 = DIRECTION ( 'NONE',  ( 0.000000000000000000, -1.000000000000000000, 0.000000000000000000 ) ) ;
#1539 = CARTESIAN_POINT ( 'NONE',  ( 68.18181818181818699, -4.172000000000000597, 0.000000000000000000 ) ) ;
#1540 = CARTESIAN_POINT ( 'NONE',  ( 0.000000000000000000, 0.000000000000000000, -3.000000000000000000 ) ) ;
#1541 = DIRECTION ( 'NONE',  ( -1.000000000000000000, 0.000000000000000000, 0.000000000000000000 ) ) ;
#1542 = DIRECTION ( 'NONE',  ( -0.7089874389501492624, 0.7052211081716913688, 0.000000000000000000 ) ) ;
#1543 = DIRECTION ( 'NONE',  ( 0.000000000000000000, -1.000000000000000000, 0.000000000000000000 ) ) ;
#1544 = ORIENTED_EDGE ( 'NONE', *, *, #8849, .T. ) ;
#1545 = CARTESIAN_POINT ( 'NONE',  ( -6.233975306307046963E-13, 9.127583699786111282, 9.133165578109188942 ) ) ;
#1546 = EDGE_LOOP ( 'NONE', ( #9703, #16962, #9143, #10092 ) ) ;
#1547 = CARTESIAN_POINT ( 'NONE',  ( 0.000000000000000000, 0.000000000000000000, 0.000000000000000000 ) ) ;
#1548 = ORIENTED_EDGE ( 'NONE', *, *, #18401, .F. ) ;
#1549 = VERTEX_POINT ( 'NONE', #6112 ) ;
#1550 = DIRECTION ( 'NONE',  ( 0.000000000000000000, -1.000000000000000000, 0.000000000000000000 ) ) ;
#1551 = CARTESIAN_POINT ( 'NONE',  ( 6.809999908187194197E-13, -9.988891130263535700, -9.559589141758145558 ) ) ;
#1552 = ADVANCED_FACE ( 'NONE', ( #13554 ), #19163, .F. ) ;
#1553 = DIRECTION ( 'NONE',  ( -1.000000000000000000, -0.000000000000000000, -0.000000000000000000 ) ) ;
#1554 = PLANE ( 'NONE',  #19356 ) ;
#1555 = CARTESIAN_POINT ( 'NONE',  ( -1.499999999999999556, 0.000000000000000000, 6.000000000000000000 ) ) ;
#1556 = DIRECTION ( 'NONE',  ( -1.000000000000000000, 0.000000000000000000, 0.000000000000000000 ) ) ;
#1557 = ORIENTED_EDGE ( 'NONE', *, *, #13534, .F. ) ;
#1558 = AXIS2_PLACEMENT_3D ( 'NONE', #10312, #2519, #8487 ) ;
#1559 = EDGE_CURVE ( 'NONE', #12121, #3740, #20996, .T. ) ;
#1560 = ADVANCED_FACE ( 'NONE', ( #4039 ), #1263, .T. ) ;
#1561 = ORIENTED_EDGE ( 'NONE', *, *, #19881, .T. ) ;
#1562 = CYLINDRICAL_SURFACE ( 'NONE', #8249, 1.000000000000000888 ) ;
#1563 = DIRECTION ( 'NONE',  ( -1.000000000000000000, 0.000000000000000000, 0.000000000000000000 ) ) ;
#1564 = DIRECTION ( 'NONE',  ( -1.000000000000000000, -0.000000000000000000, -0.000000000000000000 ) ) ;
#1565 = CARTESIAN_POINT ( 'NONE',  ( 17.15242344757784210, 8.297343789534778580, 4.632629386303498187 ) ) ;
#1566 = CYLINDRICAL_SURFACE ( 'NONE', #1355, 6.050000000006051870 ) ;
#1567 = ORIENTED_EDGE ( 'NONE', *, *, #13985, .T. ) ;
#1568 = DIRECTION ( 'NONE',  ( -0.000000000000000000, -0.000000000000000000, -1.000000000000000000 ) ) ;
#1569 = DIRECTION ( 'NONE',  ( -1.000000000000000000, 0.000000000000000000, 0.000000000000000000 ) ) ;
#1570 = ORIENTED_EDGE ( 'NONE', *, *, #8432, .F. ) ;
#1571 = ORIENTED_EDGE ( 'NONE', *, *, #1917, .T. ) ;
#1572 = CARTESIAN_POINT ( 'NONE',  ( 6.809999908187194197E-13, -9.988891130263535700, 10.70674201446023233 ) ) ;
#1573 = CARTESIAN_POINT ( 'NONE',  ( 9.499999999999790390, 3.086737114213260025, 9.306742014460233747 ) ) ;
#1574 = ORIENTED_EDGE ( 'NONE', *, *, #251, .T. ) ;
#1575 = EDGE_LOOP ( 'NONE', ( #4889, #17601, #15027, #17100, #10679, #23520 ) ) ;
#1576 = SHAPE_REPRESENTATION_RELATIONSHIP ( 'NONE' , 'NONE' ,  #17018, #13375 ) ;
#1577 = AXIS2_PLACEMENT_3D ( 'NONE', #9140, #24039, #14752 ) ;
#1578 = CARTESIAN_POINT ( 'NONE',  ( 23.00000000000000000, 0.000000000000000000, 0.000000000000000000 ) ) ;
#1579 = LINE ( 'NONE', #8996, #7236 ) ;
#1580 = ADVANCED_FACE ( 'NONE', ( #632 ), #15227, .F. ) ;
#1581 = DIRECTION ( 'NONE',  ( -1.000000000000000000, -1.224606353822377258E-16, -0.000000000000000000 ) ) ;
#1582 = CARTESIAN_POINT ( 'NONE',  ( 15.00000000000000355, 15.50000000000000000, 19.70000000000000284 ) ) ;
#1583 = DIRECTION ( 'NONE',  ( 0.000000000000000000, 1.000000000000000000, 0.000000000000000000 ) ) ;
#1584 = ORIENTED_EDGE ( 'NONE', *, *, #16258, .F. ) ;
#1585 = ADVANCED_FACE ( 'NONE', ( #4174 ), #8044, .T. ) ;
#1586 = ADVANCED_FACE ( 'NONE', ( #6225, #7677 ), #22839, .T. ) ;
#1587 = ORIENTED_EDGE ( 'NONE', *, *, #14769, .F. ) ;
#1588 = CARTESIAN_POINT ( 'NONE',  ( 41.99999999999999289, 25.93535998569253920, -27.00000000000000000 ) ) ;
#1589 = CARTESIAN_POINT ( 'NONE',  ( -0.6269384450604889025, 9.499999999999955591, -3.500543795355101295 ) ) ;
#1590 = DIRECTION ( 'NONE',  ( 0.000000000000000000, -1.000000000000000000, 0.000000000000000000 ) ) ;
#1591 = DIRECTION ( 'NONE',  ( 0.000000000000000000, 0.000000000000000000, 1.000000000000000000 ) ) ;
#1592 = CARTESIAN_POINT ( 'NONE',  ( -7.022953521754877748, -5.102474405760673015, -7.833165578109188232 ) ) ;
#1593 = DIRECTION ( 'NONE',  ( 1.000000000000000000, 0.000000000000000000, 0.000000000000000000 ) ) ;
#1594 = ORIENTED_EDGE ( 'NONE', *, *, #7005, .T. ) ;
#1595 = CARTESIAN_POINT ( 'NONE',  ( -40.89823313241237912, -26.41789760203349502, 27.00000000000000000 ) ) ;
#1596 = VERTEX_POINT ( 'NONE', #20630 ) ;
#1597 = DIRECTION ( 'NONE',  ( 1.000000000000000000, 0.000000000000000000, 0.000000000000000000 ) ) ;
#1598 = CARTESIAN_POINT ( 'NONE',  ( 82.72727272727273373, 7.491529369508391930E-15, 0.000000000000000000 ) ) ;
#1599 = VERTEX_POINT ( 'NONE', #16960 ) ;
#1600 = DIRECTION ( 'NONE',  ( 1.000000000000000000, 0.000000000000000000, 0.000000000000000000 ) ) ;
#1601 = DIRECTION ( 'NONE',  ( 1.000000000000000000, 0.000000000000000000, 0.000000000000000000 ) ) ;
#1602 = CARTESIAN_POINT ( 'NONE',  ( 76.03431729618309021, -1.078520768856852078E-29, 5.000000000000007994 ) ) ;
#1603 = LINE ( 'NONE', #23810, #6834 ) ;
#1604 = EDGE_CURVE ( 'NONE', #12835, #16165, #10960, .T. ) ;
#1605 = AXIS2_PLACEMENT_3D ( 'NONE', #18642, #3630, #5229 ) ;
#1606 = CARTESIAN_POINT ( 'NONE',  ( 0.000000000000000000, 0.000000000000000000, 0.2999999999999990452 ) ) ;
#1607 = CARTESIAN_POINT ( 'NONE',  ( -5.622572944242077574E-13, 8.680847955711007202, -3.133165578109187610 ) ) ;
#1608 = VECTOR ( 'NONE', #17271, 1000.000000000000000 ) ;
#1609 = CARTESIAN_POINT ( 'NONE',  ( -2.935661446561384391, -9.035036904804158553, -5.459589141758144137 ) ) ;
#1610 = ORIENTED_EDGE ( 'NONE', *, *, #17130, .F. ) ;
#1611 = ORIENTED_EDGE ( 'NONE', *, *, #10765, .F. ) ;
#1612 = CARTESIAN_POINT ( 'NONE',  ( 44.99999999999998579, 50.99999999999992184, 0.000000000000000000 ) ) ;
#1613 = DIRECTION ( 'NONE',  ( -1.000000000000000000, 0.000000000000000000, 0.000000000000000000 ) ) ;
#1614 = EDGE_CURVE ( 'NONE', #16055, #16900, #21108, .T. ) ;
#1615 = DIRECTION ( 'NONE',  ( -0.000000000000000000, 0.000000000000000000, 1.000000000000000000 ) ) ;
#1616 = EDGE_CURVE ( 'NONE', #6271, #5371, #20891, .T. ) ;
#1617 = VERTEX_POINT ( 'NONE', #1955 ) ;
#1618 = DIRECTION ( 'NONE',  ( 0.000000000000000000, 0.2817325568414236758, 0.9594929736144991450 ) ) ;
#1619 = CARTESIAN_POINT ( 'NONE',  ( -36.00000000000000711, -51.00000000000000711, 0.5000000000000000000 ) ) ;
#1620 = CARTESIAN_POINT ( 'NONE',  ( 3.890962118697714531E-15, 15.50000000000000000, 19.70000000000000284 ) ) ;
#1621 = ORIENTED_EDGE ( 'NONE', *, *, #1998, .F. ) ;
#1622 = DIRECTION ( 'NONE',  ( -1.000000000000000000, -1.224606353822377258E-16, -0.000000000000000000 ) ) ;
#1623 = CARTESIAN_POINT ( 'NONE',  ( -31.74999999999995737, 0.000000000000000000, 0.000000000000000000 ) ) ;
#1624 = VECTOR ( 'NONE', #19326, 1000.000000000000000 ) ;
#1625 = DIRECTION ( 'NONE',  ( -0.000000000000000000, -0.000000000000000000, -1.000000000000000000 ) ) ;
#1626 = AXIS2_PLACEMENT_3D ( 'NONE', #11724, #6023, #13210 ) ;
#1627 = DIRECTION ( 'NONE',  ( 1.000000000000000000, 0.000000000000000000, 0.000000000000000000 ) ) ;
#1628 = ORIENTED_EDGE ( 'NONE', *, *, #1510, .T. ) ;
#1629 = EDGE_CURVE ( 'NONE', #5218, #11723, #469, .T. ) ;
#1630 = VERTEX_POINT ( 'NONE', #13288 ) ;
#1631 = ORIENTED_EDGE ( 'NONE', *, *, #13899, .T. ) ;
#1632 = EDGE_CURVE ( 'NONE', #8004, #8486, #5988, .T. ) ;
#1633 = ORIENTED_EDGE ( 'NONE', *, *, #14760, .F. ) ;
#1634 = DIRECTION ( 'NONE',  ( 1.000000000000000000, 0.000000000000000000, 0.000000000000000000 ) ) ;
#1635 = DIRECTION ( 'NONE',  ( -1.000000000000000000, -1.224606353822377258E-16, -0.000000000000000000 ) ) ;
#1636 = VERTEX_POINT ( 'NONE', #17195 ) ;
#1637 = CIRCLE ( 'NONE', #4769, 1.000000000000000888 ) ;
#1638 = TOROIDAL_SURFACE ( 'NONE', #9853, 5.999999999999999112, 1.000000000000000000 ) ;
#1639 = EDGE_CURVE ( 'NONE', #21260, #13716, #19946, .T. ) ;
#1640 = EDGE_CURVE ( 'NONE', #10789, #16240, #14868, .T. ) ;
#1641 = DIRECTION ( 'NONE',  ( -0.000000000000000000, -0.000000000000000000, -1.000000000000000000 ) ) ;
#1642 = VECTOR ( 'NONE', #14147, 1000.000000000000000 ) ;
#1643 = ORIENTED_EDGE ( 'NONE', *, *, #19336, .T. ) ;
#1644 = DIRECTION ( 'NONE',  ( 1.000000000000000000, 0.000000000000000000, 0.000000000000000000 ) ) ;
#1645 = DIRECTION ( 'NONE',  ( 0.000000000000000000, 0.000000000000000000, 1.000000000000000000 ) ) ;
#1646 = CYLINDRICAL_SURFACE ( 'NONE', #3565, 1.000000000000000000 ) ;
#1647 = DIRECTION ( 'NONE',  ( 0.000000000000000000, 0.000000000000000000, 1.000000000000000000 ) ) ;
#1648 = DIRECTION ( 'NONE',  ( -0.000000000000000000, 0.000000000000000000, 1.000000000000000000 ) ) ;
#1649 = DIRECTION ( 'NONE',  ( -1.000000000000000000, 0.000000000000000000, 0.000000000000000000 ) ) ;
#1650 = CARTESIAN_POINT ( 'NONE',  ( 23.00000000000000000, -3.205857990849673378, -11.23818298448545860 ) ) ;
#1651 = ORIENTED_EDGE ( 'NONE', *, *, #19156, .T. ) ;
#1652 = EDGE_LOOP ( 'NONE', ( #551, #12219, #17711, #13018 ) ) ;
#1653 = CARTESIAN_POINT ( 'NONE',  ( 6.222797240145152671E-13, -9.127583699786111282, 8.133165578109188942 ) ) ;
#1654 = VERTEX_POINT ( 'NONE', #6351 ) ;
#1655 = AXIS2_PLACEMENT_3D ( 'NONE', #8868, #3266, #6936 ) ;
#1656 = CIRCLE ( 'NONE', #16816, 5.000000000000007994 ) ;
#1657 = AXIS2_PLACEMENT_3D ( 'NONE', #22226, #8911, #23587 ) ;
#1658 = AXIS2_PLACEMENT_3D ( 'NONE', #16702, #4265, #6090 ) ;
#1659 = ADVANCED_FACE ( 'NONE', ( #1116 ), #17559, .T. ) ;
#1660 = TOROIDAL_SURFACE ( 'NONE', #2048, 3.999999999999999112, 1.000000000000000000 ) ;
#1661 = PRODUCT_CONTEXT ( 'NONE', #5736, 'mechanical' ) ;
#1662 = AXIS2_PLACEMENT_3D ( 'NONE', #23977, #5539, #16524 ) ;
#1663 = CARTESIAN_POINT ( 'NONE',  ( 42.00000000000000000, 5.999999999999986677, 9.500000000000000000 ) ) ;
#1664 = AXIS2_PLACEMENT_3D ( 'NONE', #9285, #20289, #7569 ) ;
#1665 = ORIENTED_EDGE ( 'NONE', *, *, #10735, .T. ) ;
#1666 = VERTEX_POINT ( 'NONE', #861 ) ;
#1667 = EDGE_CURVE ( 'NONE', #2779, #5776, #3202, .T. ) ;
#1668 = DIRECTION ( 'NONE',  ( 0.1039766011667122986, 0.9945797436152711279, 0.000000000000000000 ) ) ;
#1669 = CARTESIAN_POINT ( 'NONE',  ( 8.680847955710813579, 2.820578480814259326, -8.733165578109185034 ) ) ;
#1670 = DIRECTION ( 'NONE',  ( -1.000000000000000000, -0.000000000000000000, -0.000000000000000000 ) ) ;
#1671 = DIRECTION ( 'NONE',  ( -0.000000000000000000, -0.000000000000000000, -1.000000000000000000 ) ) ;
#1672 = FACE_OUTER_BOUND ( 'NONE', #11880, .T. ) ;
#1673 = ORIENTED_EDGE ( 'NONE', *, *, #16207, .F. ) ;
#1674 = AXIS2_PLACEMENT_3D ( 'NONE', #7386, #5708, #3387 ) ;
#1675 = AXIS2_PLACEMENT_3D ( 'NONE', #11299, #11066, #17172 ) ;
#1676 = ORIENTED_EDGE ( 'NONE', *, *, #9580, .F. ) ;
#1677 = LINE ( 'NONE', #20338, #4789 ) ;
#1678 = CARTESIAN_POINT ( 'NONE',  ( 29.00000000000000711, -29.50000000000000711, -27.00000000000000000 ) ) ;
#1679 = AXIS2_PLACEMENT_3D ( 'NONE', #16031, #7947, #15257 ) ;
#1680 = AXIS2_PLACEMENT_3D ( 'NONE', #18237, #1526, #19837 ) ;
#1681 = LINE ( 'NONE', #18165, #23121 ) ;
#1682 = DIRECTION ( 'NONE',  ( 1.000000000000000000, 0.000000000000000000, 0.000000000000000000 ) ) ;
#1683 = AXIS2_PLACEMENT_3D ( 'NONE', #21822, #16210, #16425 ) ;
#1684 = VECTOR ( 'NONE', #20156, 1000.000000000000227 ) ;
#1685 = DIRECTION ( 'NONE',  ( 0.000000000000000000, -1.000000000000000000, 0.000000000000000000 ) ) ;
#1686 = DIRECTION ( 'NONE',  ( -1.000000000000000000, 0.000000000000000000, -0.000000000000000000 ) ) ;
#1687 = CONICAL_SURFACE ( 'NONE', #23891, 5.025000000000002132, 0.7853981633974482790 ) ;
#1688 = CARTESIAN_POINT ( 'NONE',  ( 23.00000000000000000, 0.000000000000000000, 0.000000000000000000 ) ) ;
#1689 = ORIENTED_EDGE ( 'NONE', *, *, #14760, .T. ) ;
#1690 = VERTEX_POINT ( 'NONE', #23201 ) ;
#1691 = CARTESIAN_POINT ( 'NONE',  ( -9.500000000000211386, 3.086737114211961064, 8.106742014460232681 ) ) ;
#1692 = ORIENTED_EDGE ( 'NONE', *, *, #21653, .T. ) ;
#1693 = ORIENTED_EDGE ( 'NONE', *, *, #6210, .F. ) ;
#1694 = DIRECTION ( 'NONE',  ( 0.000000000000000000, 0.000000000000000000, 1.000000000000000000 ) ) ;
#1695 = AXIS2_PLACEMENT_3D ( 'NONE', #14206, #13984, #2753 ) ;
#1696 = EDGE_CURVE ( 'NONE', #13107, #13357, #4657, .T. ) ;
#1697 = VECTOR ( 'NONE', #6460, 1000.000000000000000 ) ;
#1698 = CARTESIAN_POINT ( 'NONE',  ( 33.24999999999999289, 29.50000000000000000, 14.00000000000000178 ) ) ;
#1699 = DIRECTION ( 'NONE',  ( 0.000000000000000000, 0.000000000000000000, 1.000000000000000000 ) ) ;
#1700 = EDGE_CURVE ( 'NONE', #15766, #14863, #16800, .T. ) ;
#1701 = CIRCLE ( 'NONE', #4421, 1.999999999999994449 ) ;
#1702 = AXIS2_PLACEMENT_3D ( 'NONE', #16398, #12268, #3480 ) ;
#1703 = CIRCLE ( 'NONE', #3643, 5.025000000000002132 ) ;
#1704 = DIRECTION ( 'NONE',  ( -1.000000000000000000, 0.000000000000000000, 0.000000000000000000 ) ) ;
#1705 = CARTESIAN_POINT ( 'NONE',  ( -20.85000000000000142, -15.03999999999999915, -25.00000000000000000 ) ) ;
#1706 = AXIS2_PLACEMENT_3D ( 'NONE', #9128, #1581, #13027 ) ;
#1707 =( REPRESENTATION_RELATIONSHIP ('NONE','NONE', #21748, #23456 ) REPRESENTATION_RELATIONSHIP_WITH_TRANSFORMATION ( #772 )SHAPE_REPRESENTATION_RELATIONSHIP( ) );
#1708 = CARTESIAN_POINT ( 'NONE',  ( 0.000000000000000000, 0.000000000000000000, 4.000000000000000000 ) ) ;
#1709 = CARTESIAN_POINT ( 'NONE',  ( -41.00000000000000000, 6.000000000000000888, 11.00000000000000000 ) ) ;
#1710 = LINE ( 'NONE', #20149, #13741 ) ;
#1711 = DIRECTION ( 'NONE',  ( 1.000000000000000000, 0.000000000000000000, 0.000000000000000000 ) ) ;
#1712 = CARTESIAN_POINT ( 'NONE',  ( 5.365059087799946447, -7.384370330706356178, -10.33316557810919001 ) ) ;
#1713 = VECTOR ( 'NONE', #5900, 1000.000000000000000 ) ;
#1714 = CARTESIAN_POINT ( 'NONE',  ( -34.00000000000000000, -3.851859888774471706E-31, 11.00000000000000000 ) ) ;
#1715 =( BOUNDED_CURVE ( )  B_SPLINE_CURVE ( 2, ( #15462, #7876, #15329, #22802, #22925, #6308, #6084, #11917, #13525, #19261, #4254 ),
 .UNSPECIFIED., .F., .T. ) 
 B_SPLINE_CURVE_WITH_KNOTS ( ( 3, 2, 2, 2, 2, 3 ),
 ( 0.6000000000000000888, 0.6200000000000001066, 0.6400000000000001243, 0.6600000000000001421, 0.6800000000000001599, 0.7000000000000000666 ),
 .UNSPECIFIED. ) 
 CURVE ( )  GEOMETRIC_REPRESENTATION_ITEM ( )  RATIONAL_B_SPLINE_CURVE ( ( 0.9999999999999997780, 0.9510565162951537532, 1.000000000000000000, 0.9510565162951535312, 1.000000000000000000, 0.9510565162951535312, 1.000000000000000000, 0.9510565162951535312, 1.000000000000000000, 0.9510565162951533091, 1.000000000000000222 ) ) 
 REPRESENTATION_ITEM ( '' )  );
#1716 = ORIENTED_EDGE ( 'NONE', *, *, #21342, .F. ) ;
#1717 = EDGE_CURVE ( 'NONE', #3810, #3246, #9387, .T. ) ;
#1718 = CARTESIAN_POINT ( 'NONE',  ( -14.99999999999999822, -6.045577542124163753E-21, 9.499999999999994671 ) ) ;
#1719 = ORIENTED_EDGE ( 'NONE', *, *, #13137, .T. ) ;
#1720 = CARTESIAN_POINT ( 'NONE',  ( 65.27272727272728048, 7.491529369508391930E-15, 0.000000000000000000 ) ) ;
#1721 = VECTOR ( 'NONE', #15643, 1000.000000000000000 ) ;
#1722 = AXIS2_PLACEMENT_3D ( 'NONE', #17393, #9685, #13358 ) ;
#1723 = ORIENTED_EDGE ( 'NONE', *, *, #20066, .T. ) ;
#1724 = CARTESIAN_POINT ( 'NONE',  ( 8.076302169966863786, -3.241261634297124772, -12.50000000000002309 ) ) ;
#1725 = EDGE_CURVE ( 'NONE', #18312, #13651, #12521, .T. ) ;
#1726 = DIRECTION ( 'NONE',  ( -1.000000000000000000, -0.000000000000000000, -0.000000000000000000 ) ) ;
#1727 = AXIS2_PLACEMENT_3D ( 'NONE', #14130, #21593, #12298 ) ;
#1728 = EDGE_CURVE ( 'NONE', #3850, #13548, #17943, .T. ) ;
#1729 = CARTESIAN_POINT ( 'NONE',  ( -20.84999999999999787, 16.67999999999985405, 14.50000000000000000 ) ) ;
#1730 = EDGE_CURVE ( 'NONE', #13078, #17416, #5140, .T. ) ;
#1731 = EDGE_CURVE ( 'NONE', #21393, #3703, #7463, .T. ) ;
#1732 = CARTESIAN_POINT ( 'NONE',  ( 2.935661446561383503, 9.035036904804158553, -10.45958914175814414 ) ) ;
#1733 = ORIENTED_EDGE ( 'NONE', *, *, #22450, .T. ) ;
#1734 = AXIS2_PLACEMENT_3D ( 'NONE', #10098, #17317, #6473 ) ;
#1735 = ORIENTED_EDGE ( 'NONE', *, *, #1616, .T. ) ;
#1736 = CARTESIAN_POINT ( 'NONE',  ( 0.000000000000000000, 0.000000000000000000, 15.50000000000000000 ) ) ;
#1737 = CIRCLE ( 'NONE', #2110, 1.999999999999994449 ) ;
#1738 = DIRECTION ( 'NONE',  ( -1.000000000000000000, -0.000000000000000000, -0.000000000000000000 ) ) ;
#1739 = CIRCLE ( 'NONE', #13415, 4.000000000000000000 ) ;
#1740 = ORIENTED_EDGE ( 'NONE', *, *, #2156, .T. ) ;
#1741 = DIRECTION ( 'NONE',  ( -1.000000000000000000, 0.000000000000000000, 0.000000000000000000 ) ) ;
#1742 = DIRECTION ( 'NONE',  ( -1.000000000000000000, -0.000000000000000000, -0.000000000000000000 ) ) ;
#1743 = EDGE_CURVE ( 'NONE', #8495, #13101, #14798, .T. ) ;
#1744 = CARTESIAN_POINT ( 'NONE',  ( 84.76159002345582394, 5.000000000000015987, 0.000000000000000000 ) ) ;
#1745 = EDGE_LOOP ( 'NONE', ( #9840, #20300, #22621, #13867 ) ) ;
#1746 = CARTESIAN_POINT ( 'NONE',  ( 73.42022815836234884, -9.244463733058732095E-30, 5.000000000000007994 ) ) ;
#1747 = DIRECTION ( 'NONE',  ( -1.000000000000000000, -0.000000000000000000, -0.000000000000000000 ) ) ;
#1748 = DIRECTION ( 'NONE',  ( 1.000000000000000000, 0.000000000000000000, 0.000000000000000000 ) ) ;
#1749 = AXIS2_PLACEMENT_3D ( 'NONE', #13199, #13791, #20552 ) ;
#1750 = VECTOR ( 'NONE', #2488, 1000.000000000000000 ) ;
#1751 = CARTESIAN_POINT ( 'NONE',  ( -6.233975306307046963E-13, 9.127583699786111282, 7.133165578109187166 ) ) ;
#1752 = ORIENTED_EDGE ( 'NONE', *, *, #9839, .F. ) ;
#1753 = EDGE_CURVE ( 'NONE', #8486, #23937, #21373, .T. ) ;
#1754 = EDGE_CURVE ( 'NONE', #8867, #15333, #13559, .T. ) ;
#1755 = CIRCLE ( 'NONE', #11457, 5.000000000000007994 ) ;
#1756 = VERTEX_POINT ( 'NONE', #1768 ) ;
#1757 = VECTOR ( 'NONE', #7727, 1000.000000000000000 ) ;
#1758 = ORIENTED_EDGE ( 'NONE', *, *, #13030, .F. ) ;
#1759 = VERTEX_POINT ( 'NONE', #56 ) ;
#1760 = CARTESIAN_POINT ( 'NONE',  ( -40.23082370883257397, -29.50000000000000711, -1.500000000000000000 ) ) ;
#1761 = COLOUR_RGB ( '',0.7921568627450980005, 0.8196078431372548767, 0.9333333333333333481 ) ;
#1762 = DIRECTION ( 'NONE',  ( 0.000000000000000000, -1.000000000000000000, 0.000000000000000000 ) ) ;
#1763 = ORIENTED_EDGE ( 'NONE', *, *, #12525, .T. ) ;
#1764 = CARTESIAN_POINT ( 'NONE',  ( -14.51962751333974033, -3.765689428759031010, -8.721787840009202597 ) ) ;
#1765 = FACE_OUTER_BOUND ( 'NONE', #1911, .T. ) ;
#1766 = VERTEX_POINT ( 'NONE', #22389 ) ;
#1767 = DIRECTION ( 'NONE',  ( 0.8757121056631642642, 0.4828336235133043886, 0.000000000000000000 ) ) ;
#1768 = CARTESIAN_POINT ( 'NONE',  ( 0.000000000000000000, -10.66755332433025316, 4.772587172891003426 ) ) ;
#1769 = CYLINDRICAL_SURFACE ( 'NONE', #23841, 9.999999999999998224 ) ;
#1770 = DIRECTION ( 'NONE',  ( 0.5735764363510424957, 0.8191520442889943521, 0.000000000000000000 ) ) ;
#1771 = VECTOR ( 'NONE', #888, 999.9999999999998863 ) ;
#1772 = DIRECTION ( 'NONE',  ( 0.000000000000000000, 1.000000000000000000, 0.000000000000000000 ) ) ;
#1773 = AXIS2_PLACEMENT_3D ( 'NONE', #14522, #7083, #8670 ) ;
#1774 = FACE_BOUND ( 'NONE', #5128, .T. ) ;
#1775 = FACE_OUTER_BOUND ( 'NONE', #16689, .T. ) ;
#1776 = CARTESIAN_POINT ( 'NONE',  ( 71.09090909090909349, 7.491529369508391930E-15, 0.000000000000000000 ) ) ;
#1777 = CARTESIAN_POINT ( 'NONE',  ( 9.301232020971131220, 6.335487896752478916E-13, -12.19876797902886700 ) ) ;
#1778 = AXIS2_PLACEMENT_3D ( 'NONE', #3582, #1532, #12969 ) ;
#1779 = AXIS2_PLACEMENT_3D ( 'NONE', #12915, #363, #7772 ) ;
#1780 = CARTESIAN_POINT ( 'NONE',  ( 6.222797240145152671E-13, -9.127583699786111282, 10.13316557810918894 ) ) ;
#1781 = ORIENTED_EDGE ( 'NONE', *, *, #14603, .F. ) ;
#1782 = EDGE_CURVE ( 'NONE', #21873, #12980, #12739, .T. ) ;
#1783 = PRODUCT_CONTEXT ( 'NONE', #18992, 'mechanical' ) ;
#1784 = DIRECTION ( 'NONE',  ( 0.4828336235133042775, 0.8757121056631643752, 0.000000000000000000 ) ) ;
#1785 = VERTEX_POINT ( 'NONE', #3471 ) ;
#1786 = VERTEX_POINT ( 'NONE', #10884 ) ;
#1787 = DIRECTION ( 'NONE',  ( 0.000000000000000000, 0.000000000000000000, -1.000000000000000000 ) ) ;
#1788 = CARTESIAN_POINT ( 'NONE',  ( 8.680847955711007202, 5.912916378492122225E-13, -10.63316557810918894 ) ) ;
#1789 = CIRCLE ( 'NONE', #17764, 4.999999999999997335 ) ;
#1790 =( GEOMETRIC_REPRESENTATION_CONTEXT ( 3 ) GLOBAL_UNCERTAINTY_ASSIGNED_CONTEXT ( ( #18890 ) ) GLOBAL_UNIT_ASSIGNED_CONTEXT ( ( #17818, #17936, #22312 ) ) REPRESENTATION_CONTEXT ( 'NONE', 'WORKASPACE' ) );
#1791 = AXIS2_PLACEMENT_3D ( 'NONE', #22443, #18538, #18756 ) ;
#1792 = ORIENTED_EDGE ( 'NONE', *, *, #21256, .F. ) ;
#1793 = LINE ( 'NONE', #14818, #21607 ) ;
#1794 = LINE ( 'NONE', #20329, #7612 ) ;
#1795 = DIRECTION ( 'NONE',  ( 0.000000000000000000, 0.000000000000000000, -1.000000000000000000 ) ) ;
#1796 = CARTESIAN_POINT ( 'NONE',  ( 30.31394790604173295, -39.41330121100981643, 11.00000000000000000 ) ) ;
#1797 = ORIENTED_EDGE ( 'NONE', *, *, #9368, .T. ) ;
#1798 = CIRCLE ( 'NONE', #1414, 50.00000000000000000 ) ;
#1799 = AXIS2_PLACEMENT_3D ( 'NONE', #5246, #12672, #12315 ) ;
#1800 = DIRECTION ( 'NONE',  ( -0.000000000000000000, -0.000000000000000000, -1.000000000000000000 ) ) ;
#1801 = EDGE_CURVE ( 'NONE', #8729, #12142, #22144, .T. ) ;
#1802 = ORIENTED_EDGE ( 'NONE', *, *, #5103, .T. ) ;
#1803 = CARTESIAN_POINT ( 'NONE',  ( -5.871322893123449127, -8.081182679344781405, -7.359589141758142716 ) ) ;
#1804 = DIRECTION ( 'NONE',  ( 0.000000000000000000, -1.000000000000000000, 0.000000000000000000 ) ) ;
#1805 = CYLINDRICAL_SURFACE ( 'NONE', #12978, 14.99999999999999822 ) ;
#1806 = CARTESIAN_POINT ( 'NONE',  ( 0.000000000000000000, 15.03999999999999915, 25.00000000000000000 ) ) ;
#1807 = CARTESIAN_POINT ( 'NONE',  ( -36.00000000000000711, -51.00000000000000711, 0.5000000000000004441 ) ) ;
#1808 = EDGE_CURVE ( 'NONE', #11482, #23301, #22258, .T. ) ;
#1809 = DIRECTION ( 'NONE',  ( 0.000000000000000000, 0.2817325568414237313, 0.9594929736144991450 ) ) ;
#1810 = CARTESIAN_POINT ( 'NONE',  ( -6.822232771736903637E-13, 9.988891130263535700, -9.706742014460232326 ) ) ;
#1811 = AXIS2_PLACEMENT_3D ( 'NONE', #6810, #8966, #22178 ) ;
#1812 = CARTESIAN_POINT ( 'NONE',  ( 0.000000000000000000, 0.000000000000000000, 0.000000000000000000 ) ) ;
#1813 = VERTEX_POINT ( 'NONE', #22508 ) ;
#1814 = VECTOR ( 'NONE', #14793, 1000.000000000000000 ) ;
#1815 = ORIENTED_EDGE ( 'NONE', *, *, #14801, .F. ) ;
#1816 = ADVANCED_FACE ( 'NONE', ( #18965 ), #9766, .F. ) ;
#1817 = CARTESIAN_POINT ( 'NONE',  ( 9.500000000000000000, 6.470877716354879437E-13, 7.206742014460234103 ) ) ;
#1818 = VERTEX_POINT ( 'NONE', #11858 ) ;
#1819 = VERTEX_POINT ( 'NONE', #19329 ) ;
#1820 = SHAPE_REPRESENTATION_RELATIONSHIP ( 'NONE' , 'NONE' ,  #15290, #22430 ) ;
#1821 = AXIS2_PLACEMENT_3D ( 'NONE', #20514, #7782, #20738 ) ;
#1822 = PRESENTATION_LAYER_ASSIGNMENT (  '', '', ( #15439 ) ) ;
#1823 = ORIENTED_EDGE ( 'NONE', *, *, #20698, .T. ) ;
#1824 = DIRECTION ( 'NONE',  ( -1.000000000000000000, 0.000000000000000000, 0.000000000000000000 ) ) ;
#1825 = DIRECTION ( 'NONE',  ( 1.000000000000000000, 0.000000000000000000, 0.000000000000000000 ) ) ;
#1826 = CARTESIAN_POINT ( 'NONE',  ( 44.99999999999998579, 50.99999999999992184, 12.50000000000000000 ) ) ;
#1827 =( NAMED_UNIT ( * ) PLANE_ANGLE_UNIT ( ) SI_UNIT ( $, .RADIAN. ) );
#1828 = DIRECTION ( 'NONE',  ( 0.000000000000000000, -1.000000000000000000, 0.000000000000000000 ) ) ;
#1829 = CIRCLE ( 'NONE', #2610, 6.050000000006051870 ) ;
#1830 = EDGE_LOOP ( 'NONE', ( #19307, #11807, #13677, #13845 ) ) ;
#1831 = DIRECTION ( 'NONE',  ( 1.000000000000000000, 0.000000000000000000, -0.000000000000000000 ) ) ;
#1832 = FACE_OUTER_BOUND ( 'NONE', #9054, .T. ) ;
#1833 = CARTESIAN_POINT ( 'NONE',  ( -17.32141611691247718, 8.728455122802976973, -3.780491077225285768 ) ) ;
#1834 = FACE_OUTER_BOUND ( 'NONE', #23408, .T. ) ;
#1835 = CARTESIAN_POINT ( 'NONE',  ( 61.48886275072855057, 6.123233995736659786E-16, -5.000000000000007994 ) ) ;
#1836 = EDGE_CURVE ( 'NONE', #5011, #7495, #302, .T. ) ;
#1837 = ADVANCED_FACE ( 'NONE', ( #9903 ), #7709, .F. ) ;
#1838 = CIRCLE ( 'NONE', #12725, 20.85000000000000497 ) ;
#1839 = ORIENTED_EDGE ( 'NONE', *, *, #12777, .T. ) ;
#1840 = DIRECTION ( 'NONE',  ( -0.000000000000000000, -0.000000000000000000, -1.000000000000000000 ) ) ;
#1841 = EDGE_LOOP ( 'NONE', ( #5037, #6701, #16418, #6702 ) ) ;
#1842 = DIRECTION ( 'NONE',  ( -1.000000000000000000, -1.224606353822377258E-16, -0.000000000000000000 ) ) ;
#1843 = DIRECTION ( 'NONE',  ( -1.000000000000000000, 0.000000000000000000, 0.000000000000000000 ) ) ;
#1844 = ORIENTED_EDGE ( 'NONE', *, *, #23123, .T. ) ;
#1845 = DIRECTION ( 'NONE',  ( 1.000000000000000000, 0.000000000000000000, 0.000000000000000000 ) ) ;
#1846 = FACE_OUTER_BOUND ( 'NONE', #6917, .T. ) ;
#1847 = DIRECTION ( 'NONE',  ( 0.000000000000000000, -1.000000000000000000, 0.000000000000000000 ) ) ;
#1848 = CARTESIAN_POINT ( 'NONE',  ( 82.72727272727273373, 4.172000000000015696, 5.109226446042767468E-16 ) ) ;
#1849 = EDGE_CURVE ( 'NONE', #17696, #2680, #10324, .T. ) ;
#1850 = CARTESIAN_POINT ( 'NONE',  ( -6.822232771736903637E-13, 9.988891130263535700, -6.559589141758143782 ) ) ;
#1851 = ORIENTED_EDGE ( 'NONE', *, *, #3843, .T. ) ;
#1852 = ORIENTED_EDGE ( 'NONE', *, *, #22143, .T. ) ;
#1853 = FACE_OUTER_BOUND ( 'NONE', #2754, .T. ) ;
#1854 = DIRECTION ( 'NONE',  ( 0.7089874389501492624, 0.7052211081716913688, 0.000000000000000000 ) ) ;
#1855 = ORIENTED_EDGE ( 'NONE', *, *, #22563, .T. ) ;
#1856 = DIRECTION ( 'NONE',  ( -0.000000000000000000, -0.000000000000000000, -1.000000000000000000 ) ) ;
#1857 = EDGE_CURVE ( 'NONE', #978, #747, #19195, .T. ) ;
#1858 = ORIENTED_EDGE ( 'NONE', *, *, #22334, .F. ) ;
#1859 = EDGE_CURVE ( 'NONE', #22027, #14408, #8326, .T. ) ;
#1860 = FACE_OUTER_BOUND ( 'NONE', #23285, .T. ) ;
#1861 = DIRECTION ( 'NONE',  ( -0.000000000000000000, -0.000000000000000000, 1.000000000000000000 ) ) ;
#1862 = CARTESIAN_POINT ( 'NONE',  ( 28.99999999999999645, 29.50000000000000000, 16.55365763086713216 ) ) ;
#1863 = VERTEX_POINT ( 'NONE', #19446 ) ;
#1864 = DIRECTION ( 'NONE',  ( 0.000000000000000000, -1.000000000000000000, 0.000000000000000000 ) ) ;
#1865 = LINE ( 'NONE', #22370, #10979 ) ;
#1866 = DIRECTION ( 'NONE',  ( 1.000000000000000000, 0.000000000000000000, -0.000000000000000000 ) ) ;
#1867 = CARTESIAN_POINT ( 'NONE',  ( 23.00000000000000000, -9.239931321968100519, -10.79948145182508057 ) ) ;
#1868 = DIRECTION ( 'NONE',  ( 0.000000000000000000, 0.000000000000000000, -1.000000000000000000 ) ) ;
#1869 = ORIENTED_EDGE ( 'NONE', *, *, #15628, .F. ) ;
#1870 = ORIENTED_EDGE ( 'NONE', *, *, #9624, .F. ) ;
#1871 = ORIENTED_EDGE ( 'NONE', *, *, #10492, .F. ) ;
#1872 = CONTEXT_DEPENDENT_SHAPE_REPRESENTATION ( #18835, #7098 ) ;
#1873 = EDGE_LOOP ( 'NONE', ( #9576, #18180 ) ) ;
#1874 = CARTESIAN_POINT ( 'NONE',  ( -9.000000000000001776, 0.000000000000000000, 12.50000000000000000 ) ) ;
#1875 = ADVANCED_FACE ( 'NONE', ( #14412 ), #23715, .F. ) ;
#1876 = LINE ( 'NONE', #5666, #10993 ) ;
#1877 = ORIENTED_EDGE ( 'NONE', *, *, #22654, .T. ) ;
#1878 = VERTEX_POINT ( 'NONE', #14301 ) ;
#1879 = DIRECTION ( 'NONE',  ( -0.5579568342432823513, 0.8298699724180977899, 0.000000000000000000 ) ) ;
#1880 = VERTEX_POINT ( 'NONE', #4936 ) ;
#1881 = CARTESIAN_POINT ( 'NONE',  ( 6.250000000000000000, -10.82531754730548279, 2.500000000000000000 ) ) ;
#1882 = EDGE_CURVE ( 'NONE', #16756, #20379, #21513, .T. ) ;
#1883 = EDGE_CURVE ( 'NONE', #3309, #18733, #15902, .T. ) ;
#1884 = CYLINDRICAL_SURFACE ( 'NONE', #13304, 11.00000000000000711 ) ;
#1885 = AXIS2_PLACEMENT_3D ( 'NONE', #19979, #1671, #21810 ) ;
#1886 = CARTESIAN_POINT ( 'NONE',  ( -0.9830802669677229932, 45.00000000000000000, 0.000000000000000000 ) ) ;
#1887 = AXIS2_PLACEMENT_3D ( 'NONE', #13091, #16993, #1879 ) ;
#1888 = CARTESIAN_POINT ( 'NONE',  ( 15.78970982176773319, -5.581464347350856947, 7.700125654604338621 ) ) ;
#1889=STYLED_ITEM('',(#24141),#2111);
#1890 = DIRECTION ( 'NONE',  ( 0.9945797436152715720, -0.1039766011667100365, 0.000000000000000000 ) ) ;
#1891 = ORIENTED_EDGE ( 'NONE', *, *, #13570, .F. ) ;
#1892 = DIRECTION ( 'NONE',  ( -0.000000000000000000, -0.000000000000000000, -1.000000000000000000 ) ) ;
#1893 = DIRECTION ( 'NONE',  ( 1.000000000000000000, 0.000000000000000000, 0.000000000000000000 ) ) ;
#1894 = DIRECTION ( 'NONE',  ( 0.7071067811865660024, 8.659560562355159656E-17, -0.7071067811865291430 ) ) ;
#1895 = ORIENTED_EDGE ( 'NONE', *, *, #22363, .F. ) ;
#1896 = ORIENTED_EDGE ( 'NONE', *, *, #13667, .T. ) ;
#1897 = CARTESIAN_POINT ( 'NONE',  ( -6.822232771736903637E-13, 9.988891130263535700, 10.55958914175814378 ) ) ;
#1898 = VERTEX_POINT ( 'NONE', #23361 ) ;
#1899 = SHAPE_DEFINITION_REPRESENTATION ( #11302, #358 ) ;
#1900 = ORIENTED_EDGE ( 'NONE', *, *, #2767, .T. ) ;
#1901 = ORIENTED_EDGE ( 'NONE', *, *, #6858, .F. ) ;
#1902 = CARTESIAN_POINT ( 'NONE',  ( 31.10231664966676135, 45.36128193761570770, 27.00000000000000000 ) ) ;
#1903 = CARTESIAN_POINT ( 'NONE',  ( -2.682529543900285862, 8.255977015246234174, -9.233165578109188587 ) ) ;
#1904 = EDGE_LOOP ( 'NONE', ( #5054, #3375 ) ) ;
#1905 = DIRECTION ( 'NONE',  ( -1.000000000000000000, 0.000000000000000000, 0.000000000000000000 ) ) ;
#1906 = FACE_OUTER_BOUND ( 'NONE', #1447, .T. ) ;
#1907 = DIRECTION ( 'NONE',  ( -1.000000000000000000, 0.000000000000000000, 0.000000000000000000 ) ) ;
#1908 = DIRECTION ( 'NONE',  ( -0.000000000000000000, -0.000000000000000000, -1.000000000000000000 ) ) ;
#1909 = VERTEX_POINT ( 'NONE', #8683 ) ;
#1910 = CARTESIAN_POINT ( 'NONE',  ( -18.50000000000000000, 0.000000000000000000, 15.50000000000000000 ) ) ;
#1911 = EDGE_LOOP ( 'NONE', ( #23621, #12603, #7007, #9760, #11729 ) ) ;
#1912 = ORIENTED_EDGE ( 'NONE', *, *, #8849, .F. ) ;
#1913 = CARTESIAN_POINT ( 'NONE',  ( -31.74999999999995737, 0.000000000000000000, 0.000000000000000000 ) ) ;
#1914 = EDGE_CURVE ( 'NONE', #2972, #11051, #21872, .T. ) ;
#1915 = CARTESIAN_POINT ( 'NONE',  ( -9.500000000000202505, 3.086737114211975275, -8.959589141758142361 ) ) ;
#1916 = CARTESIAN_POINT ( 'NONE',  ( 3.890962118697714531E-15, 15.50000000000000000, 19.70000000000000284 ) ) ;
#1917 = EDGE_CURVE ( 'NONE', #15957, #22631, #15895, .T. ) ;
#1918 = LINE ( 'NONE', #3755, #22402 ) ;
#1919 = CARTESIAN_POINT ( 'NONE',  ( 0.000000000000000000, -15.23000000000000220, -27.00000000000000000 ) ) ;
#1920 = ORIENTED_EDGE ( 'NONE', *, *, #20741, .F. ) ;
#1921 = VERTEX_POINT ( 'NONE', #15777 ) ;
#1922 = CARTESIAN_POINT ( 'NONE',  ( -7.685661446562381371, 5.583959896777970222, 12.00674201446023481 ) ) ;
#1923 = EDGE_LOOP ( 'NONE', ( #1275, #20934, #20599, #20192 ) ) ;
#1924 = ORIENTED_EDGE ( 'NONE', *, *, #2580, .T. ) ;
#1925 = CARTESIAN_POINT ( 'NONE',  ( 0.000000000000000000, 0.000000000000000000, 3.499999999999999556 ) ) ;
#1926 = ORIENTED_EDGE ( 'NONE', *, *, #16355, .T. ) ;
#1927 = FACE_OUTER_BOUND ( 'NONE', #6392, .T. ) ;
#1928 = CYLINDRICAL_SURFACE ( 'NONE', #6866, 17.87500000001787726 ) ;
#1929 = EDGE_CURVE ( 'NONE', #15351, #13407, #14721, .T. ) ;
#1930 = FACE_OUTER_BOUND ( 'NONE', #679, .T. ) ;
#1931 = CARTESIAN_POINT ( 'NONE',  ( 35.99999999999999289, -51.00000000000000711, 0.5000000000000000000 ) ) ;
#1932 = EDGE_CURVE ( 'NONE', #5961, #21357, #17854, .T. ) ;
#1933 = CARTESIAN_POINT ( 'NONE',  ( -20.85000000000000142, -15.03999999999999915, 25.00000000000000000 ) ) ;
#1934 = ADVANCED_FACE ( 'NONE', ( #10138 ), #9258, .F. ) ;
#1935 = FACE_OUTER_BOUND ( 'NONE', #4016, .T. ) ;
#1936 = CARTESIAN_POINT ( 'NONE',  ( 2.000000000000000000, 2.449293598294706414E-16, 6.000000000000000000 ) ) ;
#1937 = CARTESIAN_POINT ( 'NONE',  ( -17.52920230446416738, 9.315347328456301312, 1.925892650121555416 ) ) ;
#1938 = CARTESIAN_POINT ( 'NONE',  ( -41.50000000000000000, 28.80990663662250739, 0.000000000000000000 ) ) ;
#1939 = DIRECTION ( 'NONE',  ( 1.000000000000000000, 0.000000000000000000, 0.000000000000000000 ) ) ;
#1940 = ORIENTED_EDGE ( 'NONE', *, *, #14691, .T. ) ;
#1941 = CARTESIAN_POINT ( 'NONE',  ( -31.74999999999995737, 0.000000000000000000, 5.000000000000000888 ) ) ;
#1942 = ORIENTED_EDGE ( 'NONE', *, *, #12802, .T. ) ;
#1943 = CIRCLE ( 'NONE', #15569, 4.499999999999997335 ) ;
#1944 = CARTESIAN_POINT ( 'NONE',  ( -41.99999999999999289, 0.000000000000000000, 9.499999999999994671 ) ) ;
#1945 = ORIENTED_EDGE ( 'NONE', *, *, #4677, .F. ) ;
#1946 = DIRECTION ( 'NONE',  ( -1.000000000000000000, 0.000000000000000000, 0.000000000000000000 ) ) ;
#1947 = DIRECTION ( 'NONE',  ( 0.000000000000000000, -1.000000000000000000, 0.000000000000000000 ) ) ;
#1948 = FACE_OUTER_BOUND ( 'NONE', #16003, .T. ) ;
#1949 = EDGE_CURVE ( 'NONE', #11857, #18226, #3197, .T. ) ;
#1950 = EDGE_CURVE ( 'NONE', #7728, #6728, #1260, .T. ) ;
#1951 = CARTESIAN_POINT ( 'NONE',  ( -5.871322893123450015, -8.081182679344781405, -5.359589141758144493 ) ) ;
#1952 = VERTEX_POINT ( 'NONE', #12089 ) ;
#1953 = DIRECTION ( 'NONE',  ( 0.000000000000000000, 0.000000000000000000, 1.000000000000000000 ) ) ;
#1954 = VECTOR ( 'NONE', #16624, 1000.000000000000000 ) ;
#1955 = CARTESIAN_POINT ( 'NONE',  ( 78.94340820527399671, -1.078520768856852078E-29, 5.000000000000007994 ) ) ;
#1956 = AXIS2_PLACEMENT_3D ( 'NONE', #19696, #6516, #13830 ) ;
#1957 = EDGE_LOOP ( 'NONE', ( #3955, #1048, #9655, #3274 ) ) ;
#1958 = DIRECTION ( 'NONE',  ( -0.000000000000000000, -0.000000000000000000, -1.000000000000000000 ) ) ;
#1959 = FILL_AREA_STYLE_COLOUR ( '', #8103 ) ;
#1960 = VERTEX_POINT ( 'NONE', #10629 ) ;
#1961 = LINE ( 'NONE', #11218, #119 ) ;
#1962 = DIRECTION ( 'NONE',  ( 1.000000000000000000, 0.000000000000000000, 0.000000000000000000 ) ) ;
#1963 = CARTESIAN_POINT ( 'NONE',  ( 29.00000000000000355, -29.50000000000000000, 12.50000000000000000 ) ) ;
#1964 = EDGE_LOOP ( 'NONE', ( #23779, #15897, #2129, #17431, #20649, #21089 ) ) ;
#1965 = CYLINDRICAL_SURFACE ( 'NONE', #13252, 17.25000000000000000 ) ;
#1966 = DIRECTION ( 'NONE',  ( 1.000000000000000000, 0.000000000000000000, 0.000000000000000000 ) ) ;
#1967 = LINE ( 'NONE', #4303, #10378 ) ;
#1968 = DIRECTION ( 'NONE',  ( 0.000000000000000000, 0.000000000000000000, 1.000000000000000000 ) ) ;
#1969 = DIRECTION ( 'NONE',  ( 0.7071067811865439090, 4.816422645750986228E-14, -0.7071067811865512365 ) ) ;
#1970 = PRESENTATION_LAYER_ASSIGNMENT (  '', '', ( #10923 ) ) ;
#1971 = APPLICATION_CONTEXT ( 'automotive_design' ) ;
#1972 = ORIENTED_EDGE ( 'NONE', *, *, #9730, .T. ) ;
#1973 = PRODUCT ( 'Lag Sleeve', 'Lag Sleeve', '', ( #13112 ) ) ;
#1974 = VERTEX_POINT ( 'NONE', #2977 ) ;
#1975 = ORIENTED_EDGE ( 'NONE', *, *, #12519, .T. ) ;
#1976 = ORIENTED_EDGE ( 'NONE', *, *, #18143, .F. ) ;
#1977 = CONTEXT_DEPENDENT_SHAPE_REPRESENTATION ( #5119, #4774 ) ;
#1978 = EDGE_CURVE ( 'NONE', #22995, #9946, #10277, .T. ) ;
#1979 = ORIENTED_EDGE ( 'NONE', *, *, #630, .T. ) ;
#1980 = FACE_OUTER_BOUND ( 'NONE', #18162, .T. ) ;
#1981 = EDGE_CURVE ( 'NONE', #14771, #780, #17731, .T. ) ;
#1982 = CARTESIAN_POINT ( 'NONE',  ( -41.00000000000000000, 0.000000000000000000, 11.00000000000000000 ) ) ;
#1983 = ORIENTED_EDGE ( 'NONE', *, *, #1276, .F. ) ;
#1984 = DIRECTION ( 'NONE',  ( 0.000000000000000000, 1.000000000000000000, -0.000000000000000000 ) ) ;
#1985 = DIRECTION ( 'NONE',  ( -0.000000000000000000, -0.000000000000000000, 1.000000000000000000 ) ) ;
#1986 = ORIENTED_EDGE ( 'NONE', *, *, #9604, .F. ) ;
#1987 = DIRECTION ( 'NONE',  ( -1.000000000000000000, 0.000000000000000000, 0.000000000000000000 ) ) ;
#1988 = VECTOR ( 'NONE', #18068, 1000.000000000000227 ) ;
#1989 = DIRECTION ( 'NONE',  ( 0.8571673007021121116, 1.049727191138618449E-16, -0.5150380749100544886 ) ) ;
#1990 = CARTESIAN_POINT ( 'NONE',  ( 0.000000000000000000, 0.000000000000000000, -12.50000000000000000 ) ) ;
#1991 = CARTESIAN_POINT ( 'NONE',  ( -34.10000000000000142, -29.49999999999999645, 12.00000000000000000 ) ) ;
#1992 = DIRECTION ( 'NONE',  ( -0.8571673007021118895, 0.000000000000000000, -0.5150380749100549327 ) ) ;
#1993 = VERTEX_POINT ( 'NONE', #1395 ) ;
#1994 = CARTESIAN_POINT ( 'NONE',  ( 64.39795365981944997, 5.000000000000015099, 0.000000000000000000 ) ) ;
#1995 = FACE_OUTER_BOUND ( 'NONE', #15776, .T. ) ;
#1996 = ORIENTED_EDGE ( 'NONE', *, *, #7805, .T. ) ;
#1997 = CARTESIAN_POINT ( 'NONE',  ( 8.680847955710813579, 2.820578480814259326, 6.733165578109187699 ) ) ;
#1998 = EDGE_CURVE ( 'NONE', #19489, #8713, #8562, .T. ) ;
#1999 = ORIENTED_EDGE ( 'NONE', *, *, #12364, .F. ) ;
#2000 = SHAPE_DEFINITION_REPRESENTATION ( #14492, #8762 ) ;
#2001 = EDGE_CURVE ( 'NONE', #14761, #14835, #8507, .T. ) ;
#2002 = CIRCLE ( 'NONE', #10183, 17.87500000001787726 ) ;
#2003 = ORIENTED_EDGE ( 'NONE', *, *, #9174, .T. ) ;
#2004 = ORIENTED_EDGE ( 'NONE', *, *, #1700, .T. ) ;
#2005 = ADVANCED_FACE ( 'NONE', ( #18687 ), #9038, .F. ) ;
#2006 = AXIS2_PLACEMENT_3D ( 'NONE', #14038, #10373, #12190 ) ;
#2007 = DIRECTION ( 'NONE',  ( 0.000000000000000000, -1.000000000000000000, 0.000000000000000000 ) ) ;
#2008 = CARTESIAN_POINT ( 'NONE',  ( 6.222797240145152671E-13, -9.127583699786111282, -10.13316557810918894 ) ) ;
#2009 = ADVANCED_FACE ( 'NONE', ( #14775 ), #18650, .T. ) ;
#2010 = EDGE_CURVE ( 'NONE', #15940, #22890, #6571, .T. ) ;
#2011 = CARTESIAN_POINT ( 'NONE',  ( 0.000000000000000000, 17.26667456984545979, 4.623588898214379128 ) ) ;
#2012 = VERTEX_POINT ( 'NONE', #18451 ) ;
#2013 = CARTESIAN_POINT ( 'NONE',  ( 1.500000000000001332, 9.797174393178825657E-16, -8.000000000000000000 ) ) ;
#2014 = CARTESIAN_POINT ( 'NONE',  ( 40.77574956473004875, -27.49633847812775400, 11.00000000000000000 ) ) ;
#2015 = FACE_OUTER_BOUND ( 'NONE', #1402, .T. ) ;
#2016 = DIRECTION ( 'NONE',  ( -1.000000000000000000, -0.000000000000000000, -0.000000000000000000 ) ) ;
#2017 = ORIENTED_EDGE ( 'NONE', *, *, #19982, .T. ) ;
#2018 = CARTESIAN_POINT ( 'NONE',  ( 3.890962118697714531E-15, 15.50000000000000000, 14.70000000000000284 ) ) ;
#2019 = ORIENTED_EDGE ( 'NONE', *, *, #15607, .F. ) ;
#2020 = ORIENTED_EDGE ( 'NONE', *, *, #10962, .T. ) ;
#2021 = DIRECTION ( 'NONE',  ( -1.000000000000000000, -0.000000000000000000, -0.000000000000000000 ) ) ;
#2022 = CARTESIAN_POINT ( 'NONE',  ( -31.10231664966676846, -45.36128193761570770, 0.000000000000000000 ) ) ;
#2023 = CARTESIAN_POINT ( 'NONE',  ( 23.00000000000000000, -7.033831428820075615, -16.43291941292179459 ) ) ;
#2024 = DIRECTION ( 'NONE',  ( 0.000000000000000000, 0.000000000000000000, 1.000000000000000000 ) ) ;
#2025 = CIRCLE ( 'NONE', #17224, 8.000000000000000000 ) ;
#2026 = CIRCLE ( 'NONE', #18783, 1.000000000000000000 ) ;
#2027 = CARTESIAN_POINT ( 'NONE',  ( 7.685661446562381371, -5.583959896777971110, -5.859589141758143604 ) ) ;
#2028 = CARTESIAN_POINT ( 'NONE',  ( -7.022953521754877748, -5.102474405760673015, -11.83316557810918823 ) ) ;
#2029 = AXIS2_PLACEMENT_3D ( 'NONE', #6736, #17715, #766 ) ;
#2030 = AXIS2_PLACEMENT_3D ( 'NONE', #9842, #15202, #20975 ) ;
#2031 = VECTOR ( 'NONE', #2727, 1000.000000000000000 ) ;
#2032 = AXIS2_PLACEMENT_3D ( 'NONE', #6638, #3091, #14071 ) ;
#2033 = FILL_AREA_STYLE ('',( #8000 ) ) ;
#2034 = ORIENTED_EDGE ( 'NONE', *, *, #1149, .F. ) ;
#2035 = EDGE_CURVE ( 'NONE', #2862, #1898, #342, .T. ) ;
#2036 = VERTEX_POINT ( 'NONE', #3685 ) ;
#2037 = CIRCLE ( 'NONE', #5161, 11.22592346138681130 ) ;
#2038 = ORIENTED_EDGE ( 'NONE', *, *, #10766, .T. ) ;
#2039 = ORIENTED_EDGE ( 'NONE', *, *, #22915, .T. ) ;
#2040 = CARTESIAN_POINT ( 'NONE',  ( -5.871322893123449127, -8.081182679344781405, 9.359589141758144493 ) ) ;
#2041 = ADVANCED_FACE ( 'NONE', ( #7335 ), #23947, .T. ) ;
#2042 = DIRECTION ( 'NONE',  ( 0.000000000000000000, -1.000000000000000000, 0.000000000000000000 ) ) ;
#2044 = AXIS2_PLACEMENT_3D ( 'NONE', #7281, #10690, #21927 ) ;
#2043 = DIRECTION ( 'NONE',  ( -0.000000000000000000, -0.000000000000000000, 1.000000000000000000 ) ) ;
#2045 = CARTESIAN_POINT ( 'NONE',  ( -41.00000000000000000, 5.000000000000000888, 12.00000000000000000 ) ) ;
#2046 = AXIS2_PLACEMENT_3D ( 'NONE', #7905, #4165, #4277 ) ;
#2047 = CIRCLE ( 'NONE', #18428, 11.23082370883260417 ) ;
#2048 = AXIS2_PLACEMENT_3D ( 'NONE', #20013, #463, #13392 ) ;
#2049 = VECTOR ( 'NONE', #9640, 1000.000000000000000 ) ;
#2050 = ORIENTED_EDGE ( 'NONE', *, *, #7379, .T. ) ;
#2051 = CONICAL_SURFACE ( 'NONE', #11376, 4.172000000000008590, 0.9599310885968742602 ) ;
#2052 = DIRECTION ( 'NONE',  ( -1.000000000000000000, 0.000000000000000000, 0.000000000000000000 ) ) ;
#2053 = FILL_AREA_STYLE ('',( #11296 ) ) ;
#2054 = CARTESIAN_POINT ( 'NONE',  ( 20.84999999999999432, -15.04000000000000448, -27.00000000000000000 ) ) ;
#2055 = CONICAL_SURFACE ( 'NONE', #21569, 5.000000000000007994, 0.9599310885968855844 ) ;
#2056 = CARTESIAN_POINT ( 'NONE',  ( -16.68233279685676607, 7.225448002938851033, -6.184784653374926222 ) ) ;
#2057 = SHAPE_REPRESENTATION ( 'Lag Sleeve', ( #8005 ), #21672 ) ;
#2058 = DIRECTION ( 'NONE',  ( 0.5735764363510427177, -0.8191520442889941300, 1.003171929053527705E-16 ) ) ;
#2059 = ORIENTED_EDGE ( 'NONE', *, *, #2375, .T. ) ;
#2060 = LINE ( 'NONE', #9357, #23600 ) ;
#2061 = ORIENTED_EDGE ( 'NONE', *, *, #14810, .F. ) ;
#2062 = LINE ( 'NONE', #16946, #2122 ) ;
#2063 = ORIENTED_EDGE ( 'NONE', *, *, #7829, .T. ) ;
#2064 = VECTOR ( 'NONE', #6177, 1000.000000000000000 ) ;
#2065 = EDGE_CURVE ( 'NONE', #12301, #23300, #19435, .T. ) ;
#2066 = DIRECTION ( 'NONE',  ( 0.5735764363510427177, -0.8191520442889941300, 1.003171929053527705E-16 ) ) ;
#2067 = CIRCLE ( 'NONE', #16488, 10.49999999999999822 ) ;
#2068 = EDGE_LOOP ( 'NONE', ( #7368, #2890, #16000, #16433 ) ) ;
#2069 = VECTOR ( 'NONE', #15183, 999.9999999999998863 ) ;
#2070 = DIRECTION ( 'NONE',  ( -1.000000000000000000, -1.776356839400250465E-15, 0.000000000000000000 ) ) ;
#2071 = AXIS2_PLACEMENT_3D ( 'NONE', #670, #21877, #7103 ) ;
#2072 = DIRECTION ( 'NONE',  ( -1.000000000000000000, -1.224606353822377258E-16, -0.000000000000000000 ) ) ;
#2073 = EDGE_CURVE ( 'NONE', #4920, #12366, #11598, .T. ) ;
#2074 = CIRCLE ( 'NONE', #7144, 1.999999999999994449 ) ;
#2075 = DIRECTION ( 'NONE',  ( 4.613626265895764052E-16, 1.000000000000000000, 0.000000000000000000 ) ) ;
#2076 = CARTESIAN_POINT ( 'NONE',  ( -5.871322893124554021, 8.081182679343978492, -10.75958914175814130 ) ) ;
#2077 = ORIENTED_EDGE ( 'NONE', *, *, #5531, .T. ) ;
#2078 = DIRECTION ( 'NONE',  ( 1.000000000000000000, 1.224606353822377258E-16, 0.000000000000000000 ) ) ;
#2079 = ORIENTED_EDGE ( 'NONE', *, *, #13110, .T. ) ;
#2080 = CARTESIAN_POINT ( 'NONE',  ( -3.008080266967722682, 45.00000000000000000, 0.000000000000000000 ) ) ;
#2081 = AXIS2_PLACEMENT_3D ( 'NONE', #6395, #8330, #13836 ) ;
#2082 = DIRECTION ( 'NONE',  ( 0.000000000000000000, 0.000000000000000000, 1.000000000000000000 ) ) ;
#2083 = CARTESIAN_POINT ( 'NONE',  ( 14.79187224938325151, 2.570168443617191212, -9.168425918763420057 ) ) ;
#2084 = VECTOR ( 'NONE', #22635, 1000.000000000000000 ) ;
#2085 = AXIS2_PLACEMENT_3D ( 'NONE', #1886, #9072, #20426 ) ;
#2086 = LINE ( 'NONE', #7683, #6615 ) ;
#2087 = AXIS2_PLACEMENT_3D ( 'NONE', #5542, #22622, #4087 ) ;
#2088 = CYLINDRICAL_SURFACE ( 'NONE', #23377, 11.68650000001168721 ) ;
#2089 = EDGE_CURVE ( 'NONE', #1507, #20489, #12936, .T. ) ;
#2090 = CIRCLE ( 'NONE', #13008, 11.68650000001168543 ) ;
#2091 = CARTESIAN_POINT ( 'NONE',  ( 41.00000000000000000, -6.000000000000015099, 11.00000000000000000 ) ) ;
#2092 = DIRECTION ( 'NONE',  ( 1.000000000000000000, 1.224606353822377258E-16, 0.000000000000000000 ) ) ;
#2093 = CARTESIAN_POINT ( 'NONE',  ( -42.00000000000000000, 4.000000000000000888, 8.500000000000000000 ) ) ;
#2094 = AXIS2_PLACEMENT_3D ( 'NONE', #7770, #13401, #475 ) ;
#2095 = ORIENTED_EDGE ( 'NONE', *, *, #2766, .T. ) ;
#2096 = DIRECTION ( 'NONE',  ( -0.5735764363510519326, 0.8191520442889876907, 1.003171929053519816E-16 ) ) ;
#2097 = EDGE_CURVE ( 'NONE', #15685, #6030, #1520, .T. ) ;
#2098 = DIRECTION ( 'NONE',  ( -1.000000000000000000, 0.000000000000000000, -0.000000000000000000 ) ) ;
#2099 = DIRECTION ( 'NONE',  ( 0.7052211081716914798, -0.7089874389501492624, 0.000000000000000000 ) ) ;
#2100 = EDGE_CURVE ( 'NONE', #1960, #17886, #2272, .T. ) ;
#2101 = CYLINDRICAL_SURFACE ( 'NONE', #17612, 5.099999999999996980 ) ;
#2102 = VERTEX_POINT ( 'NONE', #9277 ) ;
#2103 = VERTEX_POINT ( 'NONE', #16722 ) ;
#2104 = VECTOR ( 'NONE', #8033, 1000.000000000000000 ) ;
#2106 = ORIENTED_EDGE ( 'NONE', *, *, #14113, .T. ) ;
#2105 = CONICAL_SURFACE ( 'NONE', #15747, 4.172000000000008590, 0.9599310885968742602 ) ;
#2107 = DIRECTION ( 'NONE',  ( -1.000000000000000000, 0.000000000000000000, 0.000000000000000000 ) ) ;
#2108 = CARTESIAN_POINT ( 'NONE',  ( -20.85000000000000853, 15.04000000000000092, -27.00000000000000000 ) ) ;
#2109 = CIRCLE ( 'NONE', #5243, 3.500000000000003109 ) ;
#2110 = AXIS2_PLACEMENT_3D ( 'NONE', #6982, #7333, #5149 ) ;
#2111 = MANIFOLD_SOLID_BREP ( 'Chamfer1', #11216 ) ;
#2112 = CARTESIAN_POINT ( 'NONE',  ( 63.23840997654417606, -9.244463733058732095E-30, 5.000000000000007994 ) ) ;
#2113 = EDGE_LOOP ( 'NONE', ( #9487, #2649, #20729, #14313 ) ) ;
#2114 = DIRECTION ( 'NONE',  ( 0.000000000000000000, 0.000000000000000000, 1.000000000000000000 ) ) ;
#2115 = DIRECTION ( 'NONE',  ( 0.000000000000000000, 0.000000000000000000, 1.000000000000000000 ) ) ;
#2116 = ORIENTED_EDGE ( 'NONE', *, *, #476, .F. ) ;
#2117 = DIRECTION ( 'NONE',  ( -0.000000000000000000, -0.000000000000000000, -1.000000000000000000 ) ) ;
#2118 = ORIENTED_EDGE ( 'NONE', *, *, #2550, .T. ) ;
#2119 = CARTESIAN_POINT ( 'NONE',  ( 39.00000000000000000, 29.49999999999999645, 11.00000000000000000 ) ) ;
#2120 = FACE_BOUND ( 'NONE', #9016, .T. ) ;
#2121 = DIRECTION ( 'NONE',  ( 0.000000000000000000, 0.000000000000000000, -1.000000000000000000 ) ) ;
#2122 = VECTOR ( 'NONE', #22114, 1000.000000000000000 ) ;
#2123 = PLANE ( 'NONE',  #21632 ) ;
#2124 = ORIENTED_EDGE ( 'NONE', *, *, #21481, .F. ) ;
#2125 = CARTESIAN_POINT ( 'NONE',  ( -34.00000000000000000, 3.999999999999999112, 10.49999999999999822 ) ) ;
#2126 = EDGE_CURVE ( 'NONE', #2518, #18986, #3835, .T. ) ;
#2127 = CARTESIAN_POINT ( 'NONE',  ( -36.00000000000001421, 50.99999999999999289, 12.50000000000000000 ) ) ;
#2128 = EDGE_CURVE ( 'NONE', #6155, #8876, #17062, .T. ) ;
#2129 = ORIENTED_EDGE ( 'NONE', *, *, #7307, .T. ) ;
#2130 = VECTOR ( 'NONE', #11900, 1000.000000000000000 ) ;
#2131 = VERTEX_POINT ( 'NONE', #18800 ) ;
#2132 = CARTESIAN_POINT ( 'NONE',  ( -7.022953521754877748, -5.102474405760673015, 3.833165578109188676 ) ) ;
#2133 = ORIENTED_EDGE ( 'NONE', *, *, #11929, .F. ) ;
#2134 = CIRCLE ( 'NONE', #23189, 6.050000000006054535 ) ;
#2135 = PRODUCT_CONTEXT ( 'NONE', #10704, 'mechanical' ) ;
#2136 = AXIS2_PLACEMENT_3D ( 'NONE', #14845, #22314, #5593 ) ;
#2137 = ORIENTED_EDGE ( 'NONE', *, *, #2679, .F. ) ;
#2138 = EDGE_LOOP ( 'NONE', ( #1415, #8177, #14025, #21280, #15381, #5290 ) ) ;
#2139 = CARTESIAN_POINT ( 'NONE',  ( 58.00000000000000000, 7.491529369508391930E-15, 0.000000000000000000 ) ) ;
#2140 = CARTESIAN_POINT ( 'NONE',  ( -2.682529543900285862, 8.255977015246234174, -11.23316557810918859 ) ) ;
#2141 = CARTESIAN_POINT ( 'NONE',  ( 27.99999999999998934, 50.99999999999999289, 0.5000000000000000000 ) ) ;
#2142 = ORIENTED_EDGE ( 'NONE', *, *, #8463, .F. ) ;
#2143 = DIRECTION ( 'NONE',  ( -1.000000000000000000, 0.000000000000000000, 0.000000000000000000 ) ) ;
#2144 = CARTESIAN_POINT ( 'NONE',  ( 0.000000000000000000, 0.000000000000000000, 6.000000000000000000 ) ) ;
#2145 = FACE_OUTER_BOUND ( 'NONE', #1256, .T. ) ;
#2146 = CARTESIAN_POINT ( 'NONE',  ( 0.000000000000000000, 45.00000000000000000, 27.00000000000000000 ) ) ;
#2147 = DIRECTION ( 'NONE',  ( -1.000000000000000000, 0.000000000000000000, 0.000000000000000000 ) ) ;
#2148 = DIRECTION ( 'NONE',  ( 1.000000000000000000, 0.000000000000000000, 0.000000000000000000 ) ) ;
#2149 = DIRECTION ( 'NONE',  ( 0.000000000000000000, 0.000000000000000000, 1.000000000000000000 ) ) ;
#2150 = EDGE_CURVE ( 'NONE', #1494, #11408, #3918, .T. ) ;
#2151 = VECTOR ( 'NONE', #23351, 1000.000000000000000 ) ;
#2152 = ORIENTED_EDGE ( 'NONE', *, *, #6077, .T. ) ;
#2153 = DIRECTION ( 'NONE',  ( 1.000000000000000000, 0.000000000000000000, 0.000000000000000000 ) ) ;
#2154 = CIRCLE ( 'NONE', #15793, 5.000000000000007994 ) ;
#2155 = CARTESIAN_POINT ( 'NONE',  ( -41.58578643762692195, 26.57671364288190219, 12.00000000000000000 ) ) ;
#2156 = EDGE_CURVE ( 'NONE', #5794, #20283, #21385, .T. ) ;
#2157 = AXIS2_PLACEMENT_3D ( 'NONE', #12068, #14047, #19541 ) ;
#2158 = AXIS2_PLACEMENT_3D ( 'NONE', #12507, #8385, #23761 ) ;
#2159 = MANIFOLD_SOLID_BREP ( 'Boss-Extrude1', #16698 ) ;
#2160 = CARTESIAN_POINT ( 'NONE',  ( -2.935661446561384391, -9.035036904804158553, -5.459589141758144137 ) ) ;
#2161 = ADVANCED_FACE ( 'NONE', ( #13432 ), #9650, .T. ) ;
#2162 = DIRECTION ( 'NONE',  ( 0.000000000000000000, 0.000000000000000000, 1.000000000000000000 ) ) ;
#2163 = ADVANCED_FACE ( 'NONE', ( #15491, #16965, #18935, #21112, #7922, #5866, #279, #20753 ), #22959, .T. ) ;
#2164 = EDGE_LOOP ( 'NONE', ( #11800, #13425, #11091, #19291 ) ) ;
#2165 = VERTEX_POINT ( 'NONE', #17454 ) ;
#2166 =( REPRESENTATION_RELATIONSHIP ('NONE','NONE', #21748, #15290 ) REPRESENTATION_RELATIONSHIP_WITH_TRANSFORMATION ( #13311 )SHAPE_REPRESENTATION_RELATIONSHIP( ) );
#2167 = ORIENTED_EDGE ( 'NONE', *, *, #19047, .T. ) ;
#2168 = CIRCLE ( 'NONE', #14633, 8.000000000000000000 ) ;
#2169 = VERTEX_POINT ( 'NONE', #9873 ) ;
#2170 = CIRCLE ( 'NONE', #9552, 5.000000000000007994 ) ;
#2171 = VERTEX_POINT ( 'NONE', #9742 ) ;
#2172 = LINE ( 'NONE', #17044, #5315 ) ;
#2173 = VECTOR ( 'NONE', #8482, 1000.000000000000000 ) ;
#2174 = CARTESIAN_POINT ( 'NONE',  ( 3.000000000000002665, 6.000000000000000000, 98.99999999999998579 ) ) ;
#2175 = CARTESIAN_POINT ( 'NONE',  ( 29.00000000000000000, 29.50000000000000000, -3.000000000000000000 ) ) ;
#2176 = PLANE ( 'NONE',  #22806 ) ;
#2177 = DIRECTION ( 'NONE',  ( 0.000000000000000000, 0.000000000000000000, 1.000000000000000000 ) ) ;
#2178 = DIRECTION ( 'NONE',  ( 0.000000000000000000, 0.000000000000000000, -1.000000000000000000 ) ) ;
#2179 = EDGE_CURVE ( 'NONE', #20131, #14640, #17307, .T. ) ;
#2180 = CARTESIAN_POINT ( 'NONE',  ( -44.00000000000001421, 50.99999999999999289, 0.5000000000000000000 ) ) ;
#2181 = AXIS2_PLACEMENT_3D ( 'NONE', #15805, #8353, #19362 ) ;
#2182 = DIRECTION ( 'NONE',  ( -1.000000000000000000, 0.000000000000000000, 0.000000000000000000 ) ) ;
#2183 = DIRECTION ( 'NONE',  ( -0.5735764363510517105, -0.8191520442889879128, 0.000000000000000000 ) ) ;
#2184 = CARTESIAN_POINT ( 'NONE',  ( -15.09475045435787166, 4.494086555308239639, -8.407297576120608795 ) ) ;
#2185 = PRODUCT_DEFINITION_FORMATION_WITH_SPECIFIED_SOURCE ( 'ANY', '', #4982, .NOT_KNOWN. ) ;
#2186 = CARTESIAN_POINT ( 'NONE',  ( 5.078177448618336420, 1.340640987761100385E-15, -10.94716442891539643 ) ) ;
#2187 = ADVANCED_FACE ( 'NONE', ( #11322 ), #17083, .T. ) ;
#2188 = ORIENTED_EDGE ( 'NONE', *, *, #19568, .T. ) ;
#2189 = EDGE_CURVE ( 'NONE', #16661, #17696, #10053, .T. ) ;
#2190 = DIRECTION ( 'NONE',  ( -1.000000000000000000, -1.224606353822377258E-16, -0.000000000000000000 ) ) ;
#2191 = CONICAL_SURFACE ( 'NONE', #23653, 5.000000000000007994, 0.9599310885968855844 ) ;
#2192 = AXIS2_PLACEMENT_3D ( 'NONE', #8280, #15732, #23197 ) ;
#2193 = ORIENTED_EDGE ( 'NONE', *, *, #14693, .T. ) ;
#2194 = PLANE ( 'NONE',  #3303 ) ;
#2195 = ORIENTED_EDGE ( 'NONE', *, *, #5691, .T. ) ;
#2196 = ORIENTED_EDGE ( 'NONE', *, *, #23015, .F. ) ;
#2197 = CARTESIAN_POINT ( 'NONE',  ( 665.5295305079686159, 872.2216676388150063, 1283.253407838750491 ) ) ;
#2198 = DIRECTION ( 'NONE',  ( 0.000000000000000000, -1.000000000000000000, 0.000000000000000000 ) ) ;
#2199 = DIRECTION ( 'NONE',  ( 1.000000000000000000, -0.000000000000000000, -0.000000000000000000 ) ) ;
#2200 = B_SPLINE_CURVE_WITH_KNOTS ( 'NONE', 3,
 ( #12990, #3605, #16298, #14584, #11027, #7148, #23757, #23867, #20102, #12502 ),
 .UNSPECIFIED., .F., .F.,
 ( 4, 2, 2, 2, 4 ),
 ( 1.433669752132626775E-14, 0.001535707958717136149, 0.003071415917419935675, 0.004607123876122735419, 0.006142831834825534729 ),
 .UNSPECIFIED. ) ;
#2201 = CARTESIAN_POINT ( 'NONE',  ( -39.00000000000000000, 0.000000000000000000, 12.00000000000000000 ) ) ;
#2202 = PRODUCT_DEFINITION_FORMATION_WITH_SPECIFIED_SOURCE ( 'ANY', '', #9355, .NOT_KNOWN. ) ;
#2203 = CIRCLE ( 'NONE', #7252, 11.68650000001168898 ) ;
#2204 = CARTESIAN_POINT ( 'NONE',  ( 76.90909090909090651, 7.491529369508391930E-15, 0.000000000000000000 ) ) ;
#2205 = CIRCLE ( 'NONE', #10337, 5.000000000000007994 ) ;
#2206 =( BOUNDED_CURVE ( )  B_SPLINE_CURVE ( 2, ( #6720, #20148, #17834, #21842, #6846, #5122, #23446, #3421, #12544, #5252, #10836 ),
 .UNSPECIFIED., .F., .F. ) 
 B_SPLINE_CURVE_WITH_KNOTS ( ( 3, 2, 2, 2, 2, 3 ),
 ( 0.09999999999999992228, 0.1199999999999999262, 0.1399999999999999578, 0.1599999999999999756, 0.1799999999999999656, 0.2000000000000000111 ),
 .UNSPECIFIED. ) 
 CURVE ( )  GEOMETRIC_REPRESENTATION_ITEM ( )  RATIONAL_B_SPLINE_CURVE ( ( 1.000000000000000222, 0.9510565162951533091, 1.000000000000000000, 0.9510565162951535312, 1.000000000000000000, 0.9510565162951535312, 1.000000000000000000, 0.9510565162951535312, 1.000000000000000000, 0.9510565162951535312, 1.000000000000000000 ) ) 
 REPRESENTATION_ITEM ( '' )  );
#2207 = FACE_BOUND ( 'NONE', #22537, .T. ) ;
#2208 = ORIENTED_EDGE ( 'NONE', *, *, #23098, .T. ) ;
#2209 = DIRECTION ( 'NONE',  ( -1.000000000000000000, 0.000000000000000000, 0.000000000000000000 ) ) ;
#2210 = EDGE_LOOP ( 'NONE', ( #23210, #13746, #15162, #12332 ) ) ;
#2211 = DIRECTION ( 'NONE',  ( -0.000000000000000000, 0.000000000000000000, 1.000000000000000000 ) ) ;
#2212 = CIRCLE ( 'NONE', #14681, 9.000000000000000000 ) ;
#2213 = CARTESIAN_POINT ( 'NONE',  ( 2.601280481040925796, 8.616622289297277248, 79.49281377527864834 ) ) ;
#2214 = DIRECTION ( 'NONE',  ( 0.000000000000000000, -0.5406408174555871193, -0.8412535328311879779 ) ) ;
#2215 = LINE ( 'NONE', #9998, #23767 ) ;
#2216 = DIRECTION ( 'NONE',  ( -0.000000000000000000, -0.000000000000000000, -1.000000000000000000 ) ) ;
#2217 = VECTOR ( 'NONE', #21626, 1000.000000000000000 ) ;
#2218 = EDGE_CURVE ( 'NONE', #7729, #7495, #5394, .T. ) ;
#2219 = CARTESIAN_POINT ( 'NONE',  ( 10.40000000000000036, 0.000000000000000000, 5.000000000000000888 ) ) ;
#2220 = VECTOR ( 'NONE', #8223, 1000.000000000000000 ) ;
#2221 = CARTESIAN_POINT ( 'NONE',  ( 0.000000000000000000, -14.99147757894464306, 7.750000000000000000 ) ) ;
#2222 = VERTEX_POINT ( 'NONE', #16108 ) ;
#2223 = DIRECTION ( 'NONE',  ( 0.000000000000000000, 0.000000000000000000, 1.000000000000000000 ) ) ;
#2224 = CARTESIAN_POINT ( 'NONE',  ( -2.682529543900285862, 8.255977015246234174, 11.23316557810918859 ) ) ;
#2225 = LINE ( 'NONE', #17092, #22862 ) ;
#2226 = DIRECTION ( 'NONE',  ( -0.000000000000000000, -0.000000000000000000, -1.000000000000000000 ) ) ;
#2227 = ORIENTED_EDGE ( 'NONE', *, *, #2483, .F. ) ;
#2228 = ORIENTED_EDGE ( 'NONE', *, *, #5965, .F. ) ;
#2229 = ORIENTED_EDGE ( 'NONE', *, *, #13851, .T. ) ;
#2230 = ORIENTED_EDGE ( 'NONE', *, *, #20570, .F. ) ;
#2231 = DIRECTION ( 'NONE',  ( 1.000000000000000000, -0.000000000000000000, -0.000000000000000000 ) ) ;
#2232 = EDGE_CURVE ( 'NONE', #10767, #13127, #15521, .T. ) ;
#2233 = FACE_OUTER_BOUND ( 'NONE', #21494, .T. ) ;
#2234 = ORIENTED_EDGE ( 'NONE', *, *, #14427, .F. ) ;
#2235 = ADVANCED_FACE ( 'NONE', ( #8292 ), #17888, .T. ) ;
#2236 = CARTESIAN_POINT ( 'NONE',  ( 23.00000000000000000, 11.90821470209334798, -7.758837095328730449 ) ) ;
#2237 = ORIENTED_EDGE ( 'NONE', *, *, #4058, .F. ) ;
#2238 = DIRECTION ( 'NONE',  ( -1.000000000000000000, 0.000000000000000000, 0.000000000000000000 ) ) ;
#2239 = EDGE_CURVE ( 'NONE', #760, #8771, #19898, .T. ) ;
#2240 = ADVANCED_FACE ( 'NONE', ( #3172 ), #19796, .F. ) ;
#2241 = ORIENTED_EDGE ( 'NONE', *, *, #17756, .F. ) ;
#2242 = DIRECTION ( 'NONE',  ( 0.000000000000000000, -1.000000000000000000, 0.000000000000000000 ) ) ;
#2243 = DIRECTION ( 'NONE',  ( -1.000000000000000000, 0.000000000000000000, 0.000000000000000000 ) ) ;
#2244 = DIRECTION ( 'NONE',  ( -0.000000000000000000, -0.000000000000000000, -1.000000000000000000 ) ) ;
#2245 = DIRECTION ( 'NONE',  ( 0.000000000000000000, 1.000000000000000000, 0.000000000000000000 ) ) ;
#2246 = EDGE_LOOP ( 'NONE', ( #21172, #19621, #6418, #15102 ) ) ;
#2247 = CARTESIAN_POINT ( 'NONE',  ( 23.00000000000000000, -13.61176534793449200, 4.089617900950054619 ) ) ;
#2248 = CARTESIAN_POINT ( 'NONE',  ( 23.00000000000000000, 6.242160243097294448, -9.879763041175060323 ) ) ;
#2249 = CARTESIAN_POINT ( 'NONE',  ( 2.935661446562616295, -9.035036904803758873, -8.806742014460233747 ) ) ;
#2250 = DIRECTION ( 'NONE',  ( -0.000000000000000000, -0.000000000000000000, -1.000000000000000000 ) ) ;
#2251 = EDGE_LOOP ( 'NONE', ( #16893, #13515, #10774, #11568, #21685 ) ) ;
#2252 = CIRCLE ( 'NONE', #1107, 9.499999999999989342 ) ;
#2253 = VERTEX_POINT ( 'NONE', #4782 ) ;
#2254 = CARTESIAN_POINT ( 'NONE',  ( 2.682529543900284974, -8.255977015246234174, 4.233165578109187699 ) ) ;
#2255 = VECTOR ( 'NONE', #3089, 1000.000000000000000 ) ;
#2256 = VERTEX_POINT ( 'NONE', #21249 ) ;
#2257 = ORIENTED_EDGE ( 'NONE', *, *, #21456, .T. ) ;
#2258 = FACE_OUTER_BOUND ( 'NONE', #16826, .T. ) ;
#2259 = ORIENTED_EDGE ( 'NONE', *, *, #7805, .F. ) ;
#2260 = VERTEX_POINT ( 'NONE', #17564 ) ;
#2261 = CARTESIAN_POINT ( 'NONE',  ( 10.00000000000000000, 6.613092715395708453E-16, 5.400000000000001243 ) ) ;
#2262 = CARTESIAN_POINT ( 'NONE',  ( -2.682529543899159208, -8.255977015246598327, -6.033165578109189298 ) ) ;
#2263 = LINE ( 'NONE', #22411, #2886 ) ;
#2264 = ORIENTED_EDGE ( 'NONE', *, *, #19666, .F. ) ;
#2265 = DIRECTION ( 'NONE',  ( -0.7071067811865474617, 8.659560562354932858E-17, 0.7071067811865474617 ) ) ;
#2266 = CYLINDRICAL_SURFACE ( 'NONE', #20902, 9.500000000000000000 ) ;
#2267 = DIRECTION ( 'NONE',  ( 0.000000000000000000, 0.000000000000000000, -1.000000000000000000 ) ) ;
#2268 = ADVANCED_FACE ( 'NONE', ( #15986 ), #11225, .T. ) ;
#2269 = EDGE_CURVE ( 'NONE', #16460, #1636, #19673, .T. ) ;
#2270 = AXIS2_PLACEMENT_3D ( 'NONE', #15298, #4228, #9328 ) ;
#2271 = PLANE ( 'NONE',  #6171 ) ;
#2272 = CIRCLE ( 'NONE', #16691, 4.999999999999997335 ) ;
#2273 = CYLINDRICAL_SURFACE ( 'NONE', #1301, 5.000000000000000888 ) ;
#2274 = CARTESIAN_POINT ( 'NONE',  ( 19.85000000000000142, 16.67999999999999972, 13.50000000000000178 ) ) ;
#2275 = FACE_OUTER_BOUND ( 'NONE', #7200, .T. ) ;
#2276 = DIRECTION ( 'NONE',  ( -1.000000000000000000, -0.000000000000000000, -0.000000000000000000 ) ) ;
#2277 = MANIFOLD_SOLID_BREP ( '\X2\00d8\X0\4.0 (4) Diameter Hole1', #8908 ) ;
#2278 = CARTESIAN_POINT ( 'NONE',  ( 0.000000000000000000, 0.000000000000000000, 51.99999999999998579 ) ) ;
#2279 = CARTESIAN_POINT ( 'NONE',  ( 41.99999999999999289, 5.618459588085056979E-15, -10.50249999999999950 ) ) ;
#2280 = AXIS2_PLACEMENT_3D ( 'NONE', #13572, #8060, #5878 ) ;
#2281 = SURFACE_STYLE_FILL_AREA ( #227 ) ;
#2282 = ORIENTED_EDGE ( 'NONE', *, *, #755, .T. ) ;
#2283 = ORIENTED_EDGE ( 'NONE', *, *, #24097, .F. ) ;
#2284 = CARTESIAN_POINT ( 'NONE',  ( -8.680847955711007202, -5.923547351154968927E-13, 11.63316557810919072 ) ) ;
#2285 = EDGE_LOOP ( 'NONE', ( #20924, #18 ) ) ;
#2286 = DIRECTION ( 'NONE',  ( 1.000000000000000000, 0.000000000000000000, 0.000000000000000000 ) ) ;
#2287 = DIRECTION ( 'NONE',  ( -0.000000000000000000, -0.000000000000000000, -1.000000000000000000 ) ) ;
#2288 = ORIENTED_EDGE ( 'NONE', *, *, #11297, .T. ) ;
#2289 = CYLINDRICAL_SURFACE ( 'NONE', #17369, 5.000000000000000888 ) ;
#2290 = UNCERTAINTY_MEASURE_WITH_UNIT (LENGTH_MEASURE( 1.000000000000000082E-05 ), #15190, 'distance_accuracy_value', 'NONE');
#2291 = EDGE_CURVE ( 'NONE', #23011, #13651, #11954, .T. ) ;
#2292 = FACE_OUTER_BOUND ( 'NONE', #10702, .T. ) ;
#2293 = DIRECTION ( 'NONE',  ( -1.000000000000000000, -1.224606353822377258E-16, -0.000000000000000000 ) ) ;
#2294 = CARTESIAN_POINT ( 'NONE',  ( -2.024999999999999911, -45.00000000000000000, 0.000000000000000000 ) ) ;
#2295 = FACE_OUTER_BOUND ( 'NONE', #4589, .T. ) ;
#2296 = ORIENTED_EDGE ( 'NONE', *, *, #20584, .T. ) ;
#2297 = EDGE_CURVE ( 'NONE', #20703, #4215, #10886, .T. ) ;
#2298 = EDGE_CURVE ( 'NONE', #3124, #22790, #13819, .T. ) ;
#2299 = EDGE_LOOP ( 'NONE', ( #18222, #654, #11732, #15797 ) ) ;
#2300 = CARTESIAN_POINT ( 'NONE',  ( 28.27483331787888332, -41.23752903419610050, 12.00000000000000000 ) ) ;
#2301 = DIRECTION ( 'NONE',  ( -0.5735764363510517105, -0.8191520442889879128, 0.000000000000000000 ) ) ;
#2302 = ORIENTED_EDGE ( 'NONE', *, *, #2550, .F. ) ;
#2303 =( NAMED_UNIT ( * ) SI_UNIT ( $, .STERADIAN. ) SOLID_ANGLE_UNIT ( ) );
#2304 = CARTESIAN_POINT ( 'NONE',  ( 11.49999999999999822, 11.37860023611340665, 13.78561139983856521 ) ) ;
#2305 = DIRECTION ( 'NONE',  ( 0.000000000000000000, 0.000000000000000000, 1.000000000000000000 ) ) ;
#2306 = FACE_OUTER_BOUND ( 'NONE', #16209, .T. ) ;
#2307 = VERTEX_POINT ( 'NONE', #6608 ) ;
#2308 = CARTESIAN_POINT ( 'NONE',  ( -8.680847955711200825, 2.820578480813073607, -7.533165578109188409 ) ) ;
#2309 = LINE ( 'NONE', #13273, #15794 ) ;
#2310 = ORIENTED_EDGE ( 'NONE', *, *, #11767, .F. ) ;
#2311 = ORIENTED_EDGE ( 'NONE', *, *, #15135, .F. ) ;
#2312 = CARTESIAN_POINT ( 'NONE',  ( -47.34180362313354351, -5.000000000000002665, 9.500000000000000000 ) ) ;
#2313 = ORIENTED_EDGE ( 'NONE', *, *, #19331, .T. ) ;
#2314 = SHAPE_REPRESENTATION_RELATIONSHIP ( 'NONE' , 'NONE' ,  #8762, #17167 ) ;
#2315 = DIRECTION ( 'NONE',  ( -0.4828336235133043330, 0.8757121056631641531, 0.000000000000000000 ) ) ;
#2316 = ADVANCED_FACE ( 'NONE', ( #14044 ), #9136, .T. ) ;
#2317 = LINE ( 'NONE', #22827, #5172 ) ;
#2318 = TOROIDAL_SURFACE ( 'NONE', #6996, 3.999999999999999112, 1.000000000000000000 ) ;
#2319 = DIRECTION ( 'NONE',  ( 0.000000000000000000, -3.469446951953611033E-15, 1.000000000000000000 ) ) ;
#2320 = CARTESIAN_POINT ( 'NONE',  ( 40.00000000000000000, 0.000000000000000000, 0.000000000000000000 ) ) ;
#2321 = LINE ( 'NONE', #19286, #18832 ) ;
#2322 = CARTESIAN_POINT ( 'NONE',  ( 40.23082370883257397, -29.49999999999999645, -3.000000000000000000 ) ) ;
#2323 = EDGE_CURVE ( 'NONE', #6244, #208, #12242, .T. ) ;
#2324 = EDGE_CURVE ( 'NONE', #18928, #20510, #16234, .T. ) ;
#2325 = CARTESIAN_POINT ( 'NONE',  ( -41.73082370883258108, -29.50000000000000711, -1.500000000000000000 ) ) ;
#2326 = EDGE_LOOP ( 'NONE', ( #22374, #9660, #18680, #10878 ) ) ;
#2327 = ORIENTED_EDGE ( 'NONE', *, *, #869, .T. ) ;
#2328 = CARTESIAN_POINT ( 'NONE',  ( -8.523217878158652283, -3.742469342540160060, 12.19934731935375538 ) ) ;
#2329 = CIRCLE ( 'NONE', #14790, 10.00000000000000178 ) ;
#2330 = CARTESIAN_POINT ( 'NONE',  ( -9.345831411446008374, 1.026058333938473455, 12.10150359048600954 ) ) ;
#2331 = VECTOR ( 'NONE', #2058, 1000.000000000000000 ) ;
#2332 = CYLINDRICAL_SURFACE ( 'NONE', #777, 18.50000000000000000 ) ;
#2333 = DIRECTION ( 'NONE',  ( -1.000000000000000000, 0.000000000000000000, 0.000000000000000000 ) ) ;
#2334 = FACE_OUTER_BOUND ( 'NONE', #2364, .T. ) ;
#2335 = CARTESIAN_POINT ( 'NONE',  ( 7.685661446562381371, -5.583959896777971110, -7.006742014460233037 ) ) ;
#2336 = VERTEX_POINT ( 'NONE', #20258 ) ;
#2337 = CYLINDRICAL_SURFACE ( 'NONE', #5475, 5.099999999999996980 ) ;
#2338 = CARTESIAN_POINT ( 'NONE',  ( -8.680847955711007202, -5.923547351154968927E-13, 9.633165578109188942 ) ) ;
#2339 = CARTESIAN_POINT ( 'NONE',  ( 23.00000000000000000, -17.86986844953242937, 0.4282833139926502386 ) ) ;
#2340 = CARTESIAN_POINT ( 'NONE',  ( 68.76159002345582394, 7.562528597612068045E-15, 0.000000000000000000 ) ) ;
#2341 = EDGE_CURVE ( 'NONE', #20691, #13956, #16922, .T. ) ;
#2342 = DIRECTION ( 'NONE',  ( -1.000000000000000000, -1.224606353822377258E-16, -0.000000000000000000 ) ) ;
#2343 = EDGE_CURVE ( 'NONE', #20236, #19090, #10726, .T. ) ;
#2345 = VERTEX_POINT ( 'NONE', #7412 ) ;
#2344 = AXIS2_PLACEMENT_3D ( 'NONE', #24063, #20287, #7341 ) ;
#2346 = ORIENTED_EDGE ( 'NONE', *, *, #19695, .F. ) ;
#2347 = CARTESIAN_POINT ( 'NONE',  ( -9.378401895172215674, 3.550564238312661509E-15, 12.12159810482778077 ) ) ;
#2348 = EDGE_CURVE ( 'NONE', #530, #9521, #13021, .T. ) ;
#2349 = CARTESIAN_POINT ( 'NONE',  ( -9.499999999999790390, -3.086737114213257804, -12.30674201446023197 ) ) ;
#2350 = VERTEX_POINT ( 'NONE', #14751 ) ;
#2351 = DIRECTION ( 'NONE',  ( -1.000000000000000000, -0.000000000000000000, -0.000000000000000000 ) ) ;
#2352 = EDGE_LOOP ( 'NONE', ( #7318, #18959, #10120, #775 ) ) ;
#2353 = ORIENTED_EDGE ( 'NONE', *, *, #10488, .F. ) ;
#2354 = DIRECTION ( 'NONE',  ( -1.000000000000000000, -1.224606353822377258E-16, -0.000000000000000000 ) ) ;
#2355 = CARTESIAN_POINT ( 'NONE',  ( -28.99999999999999645, 29.50000000000000000, 27.00000000000000000 ) ) ;
#2356 = CARTESIAN_POINT ( 'NONE',  ( 23.00000000000000000, -3.205857990849673378, -11.23818298448545860 ) ) ;
#2357 = LINE ( 'NONE', #6148, #5599 ) ;
#2358 = AXIS2_PLACEMENT_3D ( 'NONE', #19430, #2707, #13442 ) ;
#2359 = ORIENTED_EDGE ( 'NONE', *, *, #22600, .T. ) ;
#2360 = DIRECTION ( 'NONE',  ( -0.000000000000000000, -0.000000000000000000, 1.000000000000000000 ) ) ;
#2361 = LINE ( 'NONE', #22882, #939 ) ;
#2362 = EDGE_CURVE ( 'NONE', #14734, #22998, #19952, .T. ) ;
#2363 = ORIENTED_EDGE ( 'NONE', *, *, #17695, .F. ) ;
#2364 = EDGE_LOOP ( 'NONE', ( #21509, #16238, #21427, #20211, #16671, #7867 ) ) ;
#2365 = CARTESIAN_POINT ( 'NONE',  ( 9.500000000000209610, -3.086737114211962396, 11.95958914175814591 ) ) ;
#2366 = ORIENTED_EDGE ( 'NONE', *, *, #8789, .T. ) ;
#2367 = EDGE_CURVE ( 'NONE', #14658, #9329, #8359, .T. ) ;
#2368 = VERTEX_POINT ( 'NONE', #23796 ) ;
#2369 = FACE_OUTER_BOUND ( 'NONE', #11950, .T. ) ;
#2370 = EDGE_LOOP ( 'NONE', ( #21447, #11613, #15304, #20594 ) ) ;
#2371 = ORIENTED_EDGE ( 'NONE', *, *, #21131, .T. ) ;
#2372 = ADVANCED_FACE ( 'NONE', ( #1834 ), #4869, .T. ) ;
#2373 = CARTESIAN_POINT ( 'NONE',  ( 0.000000000000000000, 15.50000000000000000, 14.70000000000000284 ) ) ;
#2374 = CARTESIAN_POINT ( 'NONE',  ( 2.682529543900284974, -8.255977015246234174, -6.233165578109188587 ) ) ;
#2375 = EDGE_CURVE ( 'NONE', #22195, #22141, #16149, .T. ) ;
#2376 = DIRECTION ( 'NONE',  ( -1.000000000000000000, 0.000000000000000000, -0.000000000000000000 ) ) ;
#2377 = COLOUR_RGB ( '',0.7921568627450980005, 0.8196078431372548767, 0.9333333333333333481 ) ;
#2378 = VERTEX_POINT ( 'NONE', #7067 ) ;
#2379 = DIRECTION ( 'NONE',  ( -0.8757121056631642642, -0.4828336235133043886, 0.000000000000000000 ) ) ;
#2380 = CARTESIAN_POINT ( 'NONE',  ( 1.999999999999994449, 45.00000000000000000, 23.99999999999999645 ) ) ;
#2381 = CARTESIAN_POINT ( 'NONE',  ( 29.00000000000000711, -29.50000000000000711, -27.00000000000000000 ) ) ;
#2382 = CIRCLE ( 'NONE', #20311, 5.000000000000007994 ) ;
#2383 = EDGE_LOOP ( 'NONE', ( #8284, #6397, #13911, #8839, #19494 ) ) ;
#2384 = FACE_OUTER_BOUND ( 'NONE', #6402, .T. ) ;
#2385 = DIRECTION ( 'NONE',  ( -1.000000000000000000, -0.000000000000000000, 0.000000000000000000 ) ) ;
#2386 = VERTEX_POINT ( 'NONE', #18420 ) ;
#2387 = CARTESIAN_POINT ( 'NONE',  ( 7.685661446562381371, -5.583959896777971110, 3.859589141758143604 ) ) ;
#2388 = CARTESIAN_POINT ( 'NONE',  ( 87.96568270381690979, 7.420530141404717394E-15, 0.000000000000000000 ) ) ;
#2389 = FACE_OUTER_BOUND ( 'NONE', #22837, .T. ) ;
#2390 = CARTESIAN_POINT ( 'NONE',  ( -7.685661446561619314, -5.583959896779019161, -5.259589141758143960 ) ) ;
#2391 = CARTESIAN_POINT ( 'NONE',  ( 8.680847955711007202, 5.912916378492122225E-13, -8.633165578109188942 ) ) ;
#2392 = EDGE_LOOP ( 'NONE', ( #9547, #17675, #22727, #3760, #19162, #21712 ) ) ;
#2393 = ORIENTED_EDGE ( 'NONE', *, *, #2852, .F. ) ;
#2394 = EDGE_LOOP ( 'NONE', ( #1474, #1527, #23306, #8204, #12895, #6035, #13576, #8407, #13705 ) ) ;
#2395 = AXIS2_PLACEMENT_3D ( 'NONE', #18417, #23688, #16451 ) ;
#2396 = EDGE_CURVE ( 'NONE', #17583, #19174, #23397, .T. ) ;
#2397 = VECTOR ( 'NONE', #20885, 1000.000000000000000 ) ;
#2398 = AXIS2_PLACEMENT_3D ( 'NONE', #21432, #18137, #10664 ) ;
#2399 = ORIENTED_EDGE ( 'NONE', *, *, #17422, .T. ) ;
#2400 = DIRECTION ( 'NONE',  ( 1.000000000000000000, 0.000000000000000000, 0.000000000000000000 ) ) ;
#2401 = EDGE_CURVE ( 'NONE', #18602, #17488, #23570, .T. ) ;
#2402 = DIRECTION ( 'NONE',  ( 0.000000000000000000, -1.000000000000000000, 0.000000000000000000 ) ) ;
#2403 = ORIENTED_EDGE ( 'NONE', *, *, #11871, .T. ) ;
#2404 = FACE_OUTER_BOUND ( 'NONE', #13751, .T. ) ;
#2405 = CARTESIAN_POINT ( 'NONE',  ( -6.822232771736903637E-13, 9.988891130263535700, -10.55958914175814378 ) ) ;
#2406 = FACE_OUTER_BOUND ( 'NONE', #9405, .T. ) ;
#2407 = FACE_OUTER_BOUND ( 'NONE', #5414, .T. ) ;
#2408 = CARTESIAN_POINT ( 'NONE',  ( -40.23082370883258108, -27.62204025492846071, -1.500000000000000000 ) ) ;
#2409 = ORIENTED_EDGE ( 'NONE', *, *, #7860, .T. ) ;
#2410 = EDGE_LOOP ( 'NONE', ( #21868, #21107, #1584, #22497 ) ) ;
#2411 = LINE ( 'NONE', #11664, #10314 ) ;
#2412 = FACE_OUTER_BOUND ( 'NONE', #10329, .T. ) ;
#2413 = AXIS2_PLACEMENT_3D ( 'NONE', #9252, #19029, #11668 ) ;
#2414 = AXIS2_PLACEMENT_3D ( 'NONE', #2606, #7943, #11853 ) ;
#2415 = DIRECTION ( 'NONE',  ( -0.000000000000000000, -0.000000000000000000, 1.000000000000000000 ) ) ;
#2416 = DIRECTION ( 'NONE',  ( -0.000000000000000000, -0.000000000000000000, -1.000000000000000000 ) ) ;
#2417 = DIRECTION ( 'NONE',  ( 0.000000000000000000, 0.000000000000000000, 1.000000000000000000 ) ) ;
#2418 = AXIS2_PLACEMENT_3D ( 'NONE', #11978, #1037, #12232 ) ;
#2419 = CARTESIAN_POINT ( 'NONE',  ( 40.00000000000000000, 29.49999999999999645, 11.00000000000000000 ) ) ;
#2420 = CARTESIAN_POINT ( 'NONE',  ( 2.935661446562616295, -9.035036904803758873, 4.806742014460232859 ) ) ;
#2421 = ORIENTED_EDGE ( 'NONE', *, *, #23736, .T. ) ;
#2422 = CARTESIAN_POINT ( 'NONE',  ( 8.680847955710813579, 2.820578480814259326, -6.733165578109187699 ) ) ;
#2423 = ORIENTED_EDGE ( 'NONE', *, *, #22502, .F. ) ;
#2424 = ORIENTED_EDGE ( 'NONE', *, *, #15034, .F. ) ;
#2425 = CARTESIAN_POINT ( 'NONE',  ( 7.685661446561619314, 5.583959896779020049, 8.259589141758144848 ) ) ;
#2426 = ADVANCED_FACE ( 'NONE', ( #5612 ), #3781, .F. ) ;
#2427 = FACE_OUTER_BOUND ( 'NONE', #120, .T. ) ;
#2428 = ADVANCED_FACE ( 'NONE', ( #8 ), #3302, .T. ) ;
#2429 = VERTEX_POINT ( 'NONE', #22330 ) ;
#2430 = DIRECTION ( 'NONE',  ( -6.162975822039154730E-33, -1.232595164407830946E-32, 0.9999999999999997780 ) ) ;
#2431 = CARTESIAN_POINT ( 'NONE',  ( -31.74999999999995737, 0.000000000000000000, 0.000000000000000000 ) ) ;
#2432 = MANIFOLD_SOLID_BREP ( 'Bore', #5036 ) ;
#2433 = CARTESIAN_POINT ( 'NONE',  ( 29.00000000000000000, 29.50000000000000355, 0.000000000000000000 ) ) ;
#2434 = CIRCLE ( 'NONE', #1674, 1.000000000000000888 ) ;
#2435 = VECTOR ( 'NONE', #726, 1000.000000000000000 ) ;
#2436 = PLANE ( 'NONE',  #19714 ) ;
#2437 = CONICAL_SURFACE ( 'NONE', #18805, 9.000000000000000000, 0.7853981633974482790 ) ;
#2438 = VECTOR ( 'NONE', #3213, 1000.000000000000000 ) ;
#2439 = CARTESIAN_POINT ( 'NONE',  ( 29.00000000000000000, 29.50000000000000000, 14.00000000000000178 ) ) ;
#2440 = AXIS2_PLACEMENT_3D ( 'NONE', #22894, #3964, #11515 ) ;
#2441 = CARTESIAN_POINT ( 'NONE',  ( -7.685661446561619314, -5.583959896779019161, -3.259589141758143516 ) ) ;
#2442 = ORIENTED_EDGE ( 'NONE', *, *, #17436, .T. ) ;
#2443 = DIRECTION ( 'NONE',  ( 1.000000000000000000, 0.000000000000000000, 0.000000000000000000 ) ) ;
#2444 = VERTEX_POINT ( 'NONE', #9108 ) ;
#2445 = DIRECTION ( 'NONE',  ( -1.000000000000000000, -0.000000000000000000, -0.000000000000000000 ) ) ;
#2446 = CARTESIAN_POINT ( 'NONE',  ( -8.133009343831700377, 4.898054503500675949, 12.01970453032984487 ) ) ;
#2447 = EDGE_CURVE ( 'NONE', #14709, #6020, #4064, .T. ) ;
#2448 = CIRCLE ( 'NONE', #1695, 1.999999999999994449 ) ;
#2449 = CARTESIAN_POINT ( 'NONE',  ( 0.000000000000000000, 0.000000000000000000, -27.00000000000000000 ) ) ;
#2450 = CARTESIAN_POINT ( 'NONE',  ( -1.984007748668716653, 8.779741040573222577, 78.74128913175751165 ) ) ;
#2451 = AXIS2_PLACEMENT_3D ( 'NONE', #11583, #10885, #15230 ) ;
#2452 = DIRECTION ( 'NONE',  ( 1.000000000000000000, 0.000000000000000000, 0.000000000000000000 ) ) ;
#2453 = VECTOR ( 'NONE', #18838, 1000.000000000000000 ) ;
#2454 = CARTESIAN_POINT ( 'NONE',  ( 84.76159002345582394, 7.562528597612068045E-15, 0.000000000000000000 ) ) ;
#2455 = CIRCLE ( 'NONE', #8684, 5.999999999999998224 ) ;
#2456 = EDGE_CURVE ( 'NONE', #15497, #14826, #10290, .T. ) ;
#2457 = VERTEX_POINT ( 'NONE', #21819 ) ;
#2458 = CARTESIAN_POINT ( 'NONE',  ( -7.685661446562381371, 5.583959896777970222, -4.006742014460233925 ) ) ;
#2459 = ORIENTED_EDGE ( 'NONE', *, *, #5391, .F. ) ;
#2460 = DIRECTION ( 'NONE',  ( -0.000000000000000000, -0.000000000000000000, -1.000000000000000000 ) ) ;
#2461 = CARTESIAN_POINT ( 'NONE',  ( 8.680847955710813579, 2.820578480814259326, 8.733165578109186811 ) ) ;
#2462 = ADVANCED_FACE ( 'NONE', ( #19872, #10388 ), #21937, .T. ) ;
#2463 = EDGE_CURVE ( 'NONE', #20705, #4173, #13404, .T. ) ;
#2464 = EDGE_CURVE ( 'NONE', #15397, #4017, #6009, .T. ) ;
#2465 = CIRCLE ( 'NONE', #20015, 2.500000000000002220 ) ;
#2466 = CYLINDRICAL_SURFACE ( 'NONE', #3774, 23.84999999999999432 ) ;
#2467 = CARTESIAN_POINT ( 'NONE',  ( 21.85000000000000497, 16.67999999999999972, 13.00000000000000178 ) ) ;
#2468 = COLOUR_RGB ( '',0.7921568627450980005, 0.8196078431372548767, 0.9333333333333333481 ) ;
#2469 = ORIENTED_EDGE ( 'NONE', *, *, #4120, .T. ) ;
#2471 = AXIS2_PLACEMENT_3D ( 'NONE', #18746, #221, #9448 ) ;
#2470 = FACE_OUTER_BOUND ( 'NONE', #21015, .T. ) ;
#2472 = CONICAL_SURFACE ( 'NONE', #2883, 5.000000000000007994, 0.9599310885968855844 ) ;
#2473 = CIRCLE ( 'NONE', #16880, 23.85000000000000497 ) ;
#2474 = CARTESIAN_POINT ( 'NONE',  ( -5.871322893123450015, -8.081182679344781405, -8.506742014460233037 ) ) ;
#2475 = ORIENTED_EDGE ( 'NONE', *, *, #1632, .T. ) ;
#2476 = AXIS2_PLACEMENT_3D ( 'NONE', #17990, #3351, #6899 ) ;
#2477 = EDGE_LOOP ( 'NONE', ( #19377, #22413, #1763, #16024 ) ) ;
#2478 = AXIS2_PLACEMENT_3D ( 'NONE', #12357, #8572, #12236 ) ;
#2479 = CIRCLE ( 'NONE', #10273, 5.099999999999996980 ) ;
#2480 = DIRECTION ( 'NONE',  ( 0.000000000000000000, 0.000000000000000000, 1.000000000000000000 ) ) ;
#2481 = AXIS2_PLACEMENT_3D ( 'NONE', #7381, #20328, #7276 ) ;
#2482 = ORIENTED_EDGE ( 'NONE', *, *, #23391, .F. ) ;
#2483 = EDGE_CURVE ( 'NONE', #23403, #20131, #5085, .T. ) ;
#2484 = ORIENTED_EDGE ( 'NONE', *, *, #19394, .T. ) ;
#2485 = CARTESIAN_POINT ( 'NONE',  ( -29.00000000000000000, 29.49999999999999645, 11.50000000000000000 ) ) ;
#2486 = CARTESIAN_POINT ( 'NONE',  ( -27.70933665152130487, -40.41277845351217479, 11.00000000000000000 ) ) ;
#2487 = DIRECTION ( 'NONE',  ( 0.000000000000000000, -1.000000000000000000, 0.000000000000000000 ) ) ;
#2488 = DIRECTION ( 'NONE',  ( -0.000000000000000000, -1.000000000000000000, -0.000000000000000000 ) ) ;
#2489 = EDGE_LOOP ( 'NONE', ( #13194, #2536 ) ) ;
#2490 = CARTESIAN_POINT ( 'NONE',  ( 9.330908268522616567, -1.784418920661929642, -11.99999999999998934 ) ) ;
#2491 = CARTESIAN_POINT ( 'NONE',  ( -28.99999999999999645, -29.50000000000000000, -3.000000000000000000 ) ) ;
#2492 = EDGE_CURVE ( 'NONE', #4092, #19904, #15180, .T. ) ;
#2493 = ORIENTED_EDGE ( 'NONE', *, *, #20043, .F. ) ;
#2494 = EDGE_CURVE ( 'NONE', #16240, #13688, #17273, .T. ) ;
#2495 = TOROIDAL_SURFACE ( 'NONE', #12999, 51.49999999999999289, 1.500000000000000000 ) ;
#2496 = ORIENTED_EDGE ( 'NONE', *, *, #3201, .F. ) ;
#2497 = CARTESIAN_POINT ( 'NONE',  ( 5.871322893123449127, 8.081182679344781405, 4.359589141758143604 ) ) ;
#2498 = ORIENTED_EDGE ( 'NONE', *, *, #8901, .T. ) ;
#2499 = CIRCLE ( 'NONE', #1348, 5.000000000000007994 ) ;
#2500 = CIRCLE ( 'NONE', #13800, 5.000000000000007994 ) ;
#2501 = AXIS2_PLACEMENT_3D ( 'NONE', #3109, #5067, #12115 ) ;
#2502 = CONICAL_SURFACE ( 'NONE', #23173, 2.024999999999999911, 0.7853981633974743692 ) ;
#2503 = ORIENTED_EDGE ( 'NONE', *, *, #2269, .F. ) ;
#2504 = ORIENTED_EDGE ( 'NONE', *, *, #3584, .F. ) ;
#2505 = VERTEX_POINT ( 'NONE', #13504 ) ;
#2506 = CARTESIAN_POINT ( 'NONE',  ( -31.74999999999995737, 6.123233995736767268E-16, -5.000000000000000888 ) ) ;
#2507 = CARTESIAN_POINT ( 'NONE',  ( -7.022953521754877748, -5.102474405760673015, -5.833165578109188232 ) ) ;
#2508 = CARTESIAN_POINT ( 'NONE',  ( 2.935661446561383503, 9.035036904804158553, 7.606742014460233570 ) ) ;
#2509 = ORIENTED_EDGE ( 'NONE', *, *, #8040, .F. ) ;
#2510 = LINE ( 'NONE', #21784, #18102 ) ;
#2511 = DIRECTION ( 'NONE',  ( 0.7071067811865292541, 8.659560562354708526E-17, -0.7071067811865658914 ) ) ;
#2512 = CYLINDRICAL_SURFACE ( 'NONE', #10316, 1.000000000000000888 ) ;
#2513 = DIRECTION ( 'NONE',  ( 0.7052211081716914798, -0.7089874389501491514, 0.000000000000000000 ) ) ;
#2514 = EDGE_LOOP ( 'NONE', ( #8664, #78 ) ) ;
#2515 = DIRECTION ( 'NONE',  ( 0.000000000000000000, 0.000000000000000000, 1.000000000000000000 ) ) ;
#2516 = DIRECTION ( 'NONE',  ( 0.000000000000000000, -1.000000000000000000, 1.295896757998780388E-15 ) ) ;
#2517 = VECTOR ( 'NONE', #18198, 1000.000000000000000 ) ;
#2518 = VERTEX_POINT ( 'NONE', #3867 ) ;
#2519 = DIRECTION ( 'NONE',  ( -0.000000000000000000, -0.000000000000000000, -1.000000000000000000 ) ) ;
#2520 = CARTESIAN_POINT ( 'NONE',  ( 7.685661446561619314, 5.583959896779020049, -8.259589141758144848 ) ) ;
#2521 = AXIS2_PLACEMENT_3D ( 'NONE', #21049, #11751, #19227 ) ;
#2522 = CIRCLE ( 'NONE', #4877, 6.050000000006050982 ) ;
#2523 = CARTESIAN_POINT ( 'NONE',  ( -30.31394790604173650, -39.41330121100982353, 12.00000000000000000 ) ) ;
#2524 = CARTESIAN_POINT ( 'NONE',  ( -8.680847955711200825, 2.820578480813073607, -5.533165578109187521 ) ) ;
#2525 = ADVANCED_FACE ( 'NONE', ( #11533 ), #19004, .T. ) ;
#2526 = VECTOR ( 'NONE', #22921, 1000.000000000000000 ) ;
#2527 = ORIENTED_EDGE ( 'NONE', *, *, #23040, .T. ) ;
#2528 = EDGE_LOOP ( 'NONE', ( #12554, #9189, #15368, #1567 ) ) ;
#2529 = CARTESIAN_POINT ( 'NONE',  ( -2.682529543900285862, 8.255977015246234174, -11.23316557810918859 ) ) ;
#2530 = CARTESIAN_POINT ( 'NONE',  ( -7.022953521755574080, 5.102474405759713783, 11.43316557810918965 ) ) ;
#2531 = EDGE_LOOP ( 'NONE', ( #20549, #17730, #15560, #7865, #23401 ) ) ;
#2532 = CARTESIAN_POINT ( 'NONE',  ( 693.7818939062835852, 873.2537211538016209, 1347.481724745927977 ) ) ;
#2533 = CIRCLE ( 'NONE', #20846, 4.499999999999997335 ) ;
#2534 = VECTOR ( 'NONE', #13156, 1000.000000000000000 ) ;
#2535 = DIRECTION ( 'NONE',  ( -1.000000000000000000, -1.224606353822377258E-16, -0.000000000000000000 ) ) ;
#2536 = ORIENTED_EDGE ( 'NONE', *, *, #21931, .F. ) ;
#2537 = CARTESIAN_POINT ( 'NONE',  ( 23.00000000000000000, 0.000000000000000000, 0.000000000000000000 ) ) ;
#2538 = UNCERTAINTY_MEASURE_WITH_UNIT (LENGTH_MEASURE( 1.000000000000000082E-05 ), #11166, 'distance_accuracy_value', 'NONE');
#2539 = VECTOR ( 'NONE', #17298, 1000.000000000000000 ) ;
#2540 = AXIS2_PLACEMENT_3D ( 'NONE', #9026, #20039, #21752 ) ;
#2541 = CARTESIAN_POINT ( 'NONE',  ( 5.626939011991881401, -6.906580693685397954, 12.50000000000000000 ) ) ;
#2542 = PLANE ( 'NONE',  #14269 ) ;
#2543 = DIRECTION ( 'NONE',  ( -0.000000000000000000, -0.000000000000000000, -1.000000000000000000 ) ) ;
#2544 = ADVANCED_FACE ( 'NONE', ( #4236 ), #9586, .F. ) ;
#2545 = ORIENTED_EDGE ( 'NONE', *, *, #15701, .T. ) ;
#2546 = CARTESIAN_POINT ( 'NONE',  ( 20.85000000000000497, 16.67999999999999972, 13.00000000000000178 ) ) ;
#2547 = CIRCLE ( 'NONE', #16181, 9.500000000000000000 ) ;
#2548 = VECTOR ( 'NONE', #19758, 1000.000000000000000 ) ;
#2549 = CARTESIAN_POINT ( 'NONE',  ( 66.72727272727273373, 7.491529369508391930E-15, 0.000000000000000000 ) ) ;
#2550 = EDGE_CURVE ( 'NONE', #21161, #21353, #17033, .T. ) ;
#2551 = CARTESIAN_POINT ( 'NONE',  ( 74.00000000000001421, -4.172000000000000597, 0.000000000000000000 ) ) ;
#2552 = DIRECTION ( 'NONE',  ( -0.000000000000000000, -0.000000000000000000, 1.000000000000000000 ) ) ;
#2553 = DIRECTION ( 'NONE',  ( 0.000000000000000000, 1.000000000000000000, 0.000000000000000000 ) ) ;
#2554 = DIRECTION ( 'NONE',  ( 0.000000000000000000, 0.000000000000000000, 1.000000000000000000 ) ) ;
#2555 = ADVANCED_FACE ( 'NONE', ( #5714 ), #11646, .F. ) ;
#2556 = ADVANCED_FACE ( 'NONE', ( #2389 ), #22543, .T. ) ;
#2557 = DIRECTION ( 'NONE',  ( -1.000000000000000000, 0.000000000000000000, 0.000000000000000000 ) ) ;
#2558 = ORIENTED_EDGE ( 'NONE', *, *, #2324, .F. ) ;
#2559 = CARTESIAN_POINT ( 'NONE',  ( -8.680847955711007202, -5.923547351154968927E-13, -3.633165578109188054 ) ) ;
#2560 = VECTOR ( 'NONE', #12453, 1000.000000000000000 ) ;
#2561 = ORIENTED_EDGE ( 'NONE', *, *, #13105, .F. ) ;
#2562 = CARTESIAN_POINT ( 'NONE',  ( -9.499999999999790390, -3.086737114213257804, 9.159589141758145203 ) ) ;
#2563 = CARTESIAN_POINT ( 'NONE',  ( -9.500000000000000000, -6.482511860946779655E-13, 12.20674201446023410 ) ) ;
#2564 = AXIS2_PLACEMENT_3D ( 'NONE', #12487, #17767, #16278 ) ;
#2565 = VERTEX_POINT ( 'NONE', #5816 ) ;
#2566 = AXIS2_PLACEMENT_3D ( 'NONE', #23828, #5410, #7108 ) ;
#2567 = CARTESIAN_POINT ( 'NONE',  ( 8.680847955711007202, 5.912916378492122225E-13, -12.63316557810918894 ) ) ;
#2568 = DIRECTION ( 'NONE',  ( -1.000000000000000000, -1.224606353822377258E-16, -0.000000000000000000 ) ) ;
#2569 = CARTESIAN_POINT ( 'NONE',  ( 0.000000000000000000, -11.55437235128774809, 1.752358929577604085 ) ) ;
#2570 = CARTESIAN_POINT ( 'NONE',  ( 40.00000000000000711, 15.50000000000000533, 19.20000000000000995 ) ) ;
#2571 = CARTESIAN_POINT ( 'NONE',  ( 41.49999999999999289, 27.79189783386526358, 27.00000000000000000 ) ) ;
#2572 = CYLINDRICAL_SURFACE ( 'NONE', #17215, 11.68650000001168721 ) ;
#2573 = EDGE_CURVE ( 'NONE', #11737, #12175, #13132, .T. ) ;
#2574 = AXIS2_PLACEMENT_3D ( 'NONE', #1504, #15768, #6625 ) ;
#2575 =( GEOMETRIC_REPRESENTATION_CONTEXT ( 3 ) GLOBAL_UNCERTAINTY_ASSIGNED_CONTEXT ( ( #3996 ) ) GLOBAL_UNIT_ASSIGNED_CONTEXT ( ( #19282, #6101, #10356 ) ) REPRESENTATION_CONTEXT ( 'NONE', 'WORKASPACE' ) );
#2576 = CARTESIAN_POINT ( 'NONE',  ( 10.49999999999999822, 0.000000000000000000, -3.499999999999999556 ) ) ;
#2577 = ORIENTED_EDGE ( 'NONE', *, *, #21567, .T. ) ;
#2578 = VECTOR ( 'NONE', #16793, 1000.000000000000000 ) ;
#2579 = EDGE_CURVE ( 'NONE', #17856, #5523, #4483, .T. ) ;
#2580 = EDGE_CURVE ( 'NONE', #18213, #14863, #7551, .T. ) ;
#2581 = AXIS2_PLACEMENT_3D ( 'NONE', #23783, #7054, #11056 ) ;
#2582 = ORIENTED_EDGE ( 'NONE', *, *, #19608, .F. ) ;
#2583 = DIRECTION ( 'NONE',  ( 0.000000000000000000, 0.000000000000000000, 1.000000000000000000 ) ) ;
#2584 = CARTESIAN_POINT ( 'NONE',  ( 0.000000000000000000, 0.000000000000000000, -12.50000000000000000 ) ) ;
#2585 = CARTESIAN_POINT ( 'NONE',  ( 9.301232020971131220, 6.335487896752478916E-13, -12.19876797902886700 ) ) ;
#2586 = FILL_AREA_STYLE_COLOUR ( '', #13983 ) ;
#2587 = CIRCLE ( 'NONE', #12309, 40.00000000000000000 ) ;
#2588 = CARTESIAN_POINT ( 'NONE',  ( -0.3972991690984661317, 8.993302502987313929, 78.01992857238796830 ) ) ;
#2589 = DIRECTION ( 'NONE',  ( 0.000000000000000000, 0.000000000000000000, 1.000000000000000000 ) ) ;
#2590 = DIRECTION ( 'NONE',  ( 1.000000000000000000, -1.156482317317871725E-15, 0.000000000000000000 ) ) ;
#2591 = ORIENTED_EDGE ( 'NONE', *, *, #7078, .T. ) ;
#2592 = CARTESIAN_POINT ( 'NONE',  ( -7.685661446562381371, 5.583959896777970222, -8.006742014460233037 ) ) ;
#2593 = ORIENTED_EDGE ( 'NONE', *, *, #9294, .T. ) ;
#2594 = LINE ( 'NONE', #4427, #4721 ) ;
#2595 = CARTESIAN_POINT ( 'NONE',  ( -2.682529543899159208, -8.255977015246598327, 6.033165578109189298 ) ) ;
#2596 = DIRECTION ( 'NONE',  ( -1.000000000000000000, -1.224606353822377258E-16, -0.000000000000000000 ) ) ;
#2597 = PRODUCT_DEFINITION_FORMATION_WITH_SPECIFIED_SOURCE ( 'ANY', '', #10186, .NOT_KNOWN. ) ;
#2598 = AXIS2_PLACEMENT_3D ( 'NONE', #2901, #19126, #4623 ) ;
#2599 = PRODUCT_DEFINITION ( 'UNKNOWN', '', #19357, #19203 ) ;
#2600 = AXIS2_PLACEMENT_3D ( 'NONE', #12832, #10982, #1748 ) ;
#2601 = EDGE_CURVE ( 'NONE', #2783, #10832, #4888, .T. ) ;
#2602 = ORIENTED_EDGE ( 'NONE', *, *, #18125, .T. ) ;
#2603 = ORIENTED_EDGE ( 'NONE', *, *, #23259, .F. ) ;
#2604 = CARTESIAN_POINT ( 'NONE',  ( -20.85000000000000853, 15.04000000000000092, 25.00000000000000000 ) ) ;
#2605 = EDGE_CURVE ( 'NONE', #9181, #1507, #17323, .T. ) ;
#2606 = CARTESIAN_POINT ( 'NONE',  ( 0.000000000000000000, 0.000000000000000000, 15.00000000000000178 ) ) ;
#2607 = VERTEX_POINT ( 'NONE', #95 ) ;
#2608 = EDGE_CURVE ( 'NONE', #5686, #5827, #22792, .T. ) ;
#2609 = EDGE_CURVE ( 'NONE', #19097, #17386, #8566, .T. ) ;
#2610 = AXIS2_PLACEMENT_3D ( 'NONE', #1867, #18815, #20770 ) ;
#2611 = FACE_OUTER_BOUND ( 'NONE', #23729, .T. ) ;
#2612 = EDGE_LOOP ( 'NONE', ( #22974, #916, #12935, #21994, #20374, #19792 ) ) ;
#2613 = ORIENTED_EDGE ( 'NONE', *, *, #22070, .T. ) ;
#2614 = FACE_OUTER_BOUND ( 'NONE', #7953, .T. ) ;
#2615 = CARTESIAN_POINT ( 'NONE',  ( 23.00000000000000000, 8.890849273385706297, -7.584660931657394300 ) ) ;
#2616 = LINE ( 'NONE', #11980, #15325 ) ;
#2617 = PRODUCT_DEFINITION_CONTEXT ( 'detailed design', #3096, 'design' ) ;
#2618 = CARTESIAN_POINT ( 'NONE',  ( 9.500000000000000000, 1.163414459189985485E-15, 12.50000000000000000 ) ) ;
#2619 = VERTEX_POINT ( 'NONE', #8458 ) ;
#2620 = CARTESIAN_POINT ( 'NONE',  ( -23.85000000000000497, 15.03999999999999915, -27.00000000000000000 ) ) ;
#2621 = CARTESIAN_POINT ( 'NONE',  ( 67.60204634018053582, 7.420530141404717394E-15, 0.000000000000000000 ) ) ;
#2622 = CARTESIAN_POINT ( 'NONE',  ( -5.871322893124554021, 8.081182679343978492, -4.759589141758143960 ) ) ;
#2623 = ORIENTED_EDGE ( 'NONE', *, *, #15364, .F. ) ;
#2624 = ORIENTED_EDGE ( 'NONE', *, *, #20392, .T. ) ;
#2625 = CARTESIAN_POINT ( 'NONE',  ( 5.871322893124553133, -8.081182679343980269, 9.759589141758143072 ) ) ;
#2626 = ORIENTED_EDGE ( 'NONE', *, *, #18380, .T. ) ;
#2627 = ORIENTED_EDGE ( 'NONE', *, *, #16032, .F. ) ;
#2628 = ORIENTED_EDGE ( 'NONE', *, *, #9981, .F. ) ;
#2629 = EDGE_CURVE ( 'NONE', #14658, #25, #12091, .T. ) ;
#2630 = DIRECTION ( 'NONE',  ( -0.000000000000000000, -0.000000000000000000, 1.000000000000000000 ) ) ;
#2631 = CARTESIAN_POINT ( 'NONE',  ( 8.680847955710813579, 2.820578480814259326, -4.733165578109188587 ) ) ;
#2632 = CARTESIAN_POINT ( 'NONE',  ( -6.822232771736904647E-13, 9.988891130263535700, 7.706742014460232326 ) ) ;
#2633 = ORIENTED_EDGE ( 'NONE', *, *, #3914, .T. ) ;
#2634 = CYLINDRICAL_SURFACE ( 'NONE', #11041, 4.249999999999996447 ) ;
#2635 = DIRECTION ( 'NONE',  ( -0.5000000000000001110, -0.8660254037844384856, 0.000000000000000000 ) ) ;
#2637 = CARTESIAN_POINT ( 'NONE',  ( 80.39795365981946418, 5.000000000000015987, 0.000000000000000000 ) ) ;
#2636 = APPLICATION_CONTEXT ( 'automotive_design' ) ;
#2638 = EDGE_CURVE ( 'NONE', #19800, #3497, #7194, .T. ) ;
#2639 = EDGE_CURVE ( 'NONE', #19544, #10731, #21631, .T. ) ;
#2640 = CARTESIAN_POINT ( 'NONE',  ( 0.000000000000000000, 45.00000000000000000, 27.00000000000000000 ) ) ;
#2641 = ORIENTED_EDGE ( 'NONE', *, *, #18003, .F. ) ;
#2642 = DIRECTION ( 'NONE',  ( 0.000000000000000000, 0.000000000000000000, -1.000000000000000000 ) ) ;
#2643 = ORIENTED_EDGE ( 'NONE', *, *, #18204, .F. ) ;
#2644 = DIRECTION ( 'NONE',  ( 0.000000000000000000, 1.000000000000000000, 0.000000000000000000 ) ) ;
#2645 = SURFACE_STYLE_FILL_AREA ( #19371 ) ;
#2646 = CARTESIAN_POINT ( 'NONE',  ( -14.91624121966758487, -1.615102390220945150, 9.367332145225624629 ) ) ;
#2647 = CARTESIAN_POINT ( 'NONE',  ( 9.000000000000000000, 1.102182119232617714E-15, 105.0000000000000000 ) ) ;
#2648 = CARTESIAN_POINT ( 'NONE',  ( 2.682529543900284974, -8.255977015246234174, -6.233165578109188587 ) ) ;
#2649 = ORIENTED_EDGE ( 'NONE', *, *, #9525, .T. ) ;
#2650 = ORIENTED_EDGE ( 'NONE', *, *, #24032, .F. ) ;
#2651 = CARTESIAN_POINT ( 'NONE',  ( -8.680847955710813579, -2.820578480814258437, 11.73316557810918859 ) ) ;
#2652 = EDGE_LOOP ( 'NONE', ( #11425, #21561, #18459, #15988 ) ) ;
#2653 = DIRECTION ( 'NONE',  ( -0.9999999089179142375, 0.0004268069395492724277, -5.204170427930405876E-18 ) ) ;
#2654 = DIRECTION ( 'NONE',  ( -1.000000000000000000, 0.000000000000000000, 0.000000000000000000 ) ) ;
#2655 = EDGE_LOOP ( 'NONE', ( #10033, #1130, #15908, #23674 ) ) ;
#2656 = DIRECTION ( 'NONE',  ( 1.000000000000000000, 0.000000000000000000, 0.000000000000000000 ) ) ;
#2657 = DIRECTION ( 'NONE',  ( 0.000000000000000000, -0.7557495743542635980, 0.6548607339452787723 ) ) ;
#2658 = AXIS2_PLACEMENT_3D ( 'NONE', #17230, #2117, #15631 ) ;
#2659 = CYLINDRICAL_SURFACE ( 'NONE', #13769, 5.000000000000000888 ) ;
#2660 = CARTESIAN_POINT ( 'NONE',  ( 0.000000000000000000, 0.000000000000000000, -12.00000000000000000 ) ) ;
#2661 = CARTESIAN_POINT ( 'NONE',  ( 5.000000000000000000, 4.685197434473818312, -1.301042606982605321E-15 ) ) ;
#2662 = ADVANCED_FACE ( 'NONE', ( #1151 ), #14586, .T. ) ;
#2663 = EDGE_LOOP ( 'NONE', ( #19558, #24041, #23179, #12475 ) ) ;
#2664 = FACE_OUTER_BOUND ( 'NONE', #20873, .T. ) ;
#2665 = EDGE_CURVE ( 'NONE', #23772, #21717, #18503, .T. ) ;
#2666 = DIRECTION ( 'NONE',  ( -1.000000000000000000, 0.000000000000000000, 0.000000000000000000 ) ) ;
#2667 = DIRECTION ( 'NONE',  ( 0.000000000000000000, -1.000000000000000000, 0.000000000000000000 ) ) ;
#2668 = DIRECTION ( 'NONE',  ( -1.000000000000000000, -0.000000000000000000, -0.000000000000000000 ) ) ;
#2669 = DIRECTION ( 'NONE',  ( -0.000000000000000000, -0.000000000000000000, -1.000000000000000000 ) ) ;
#2670 = FACE_OUTER_BOUND ( 'NONE', #7422, .T. ) ;
#2671 = CIRCLE ( 'NONE', #14339, 1.500000000000001332 ) ;
#2672 = CARTESIAN_POINT ( 'NONE',  ( 42.00000000000000000, 25.22443390181681622, -3.000000000000000000 ) ) ;
#2673 = VERTEX_POINT ( 'NONE', #5780 ) ;
#2674 = CARTESIAN_POINT ( 'NONE',  ( -8.680847955711007202, -5.923547351154968927E-13, -5.633165578109188942 ) ) ;
#2675 = VECTOR ( 'NONE', #1856, 1000.000000000000000 ) ;
#2676 = VERTEX_POINT ( 'NONE', #2108 ) ;
#2677 = DIRECTION ( 'NONE',  ( 0.000000000000000000, 1.000000000000000000, 0.000000000000000000 ) ) ;
#2678 = FACE_OUTER_BOUND ( 'NONE', #3876, .T. ) ;
#2679 = EDGE_CURVE ( 'NONE', #18077, #4837, #8764, .T. ) ;
#2680 = VERTEX_POINT ( 'NONE', #8416 ) ;
#2681 =( NAMED_UNIT ( * ) PLANE_ANGLE_UNIT ( ) SI_UNIT ( $, .RADIAN. ) );
#2682 = DIRECTION ( 'NONE',  ( 0.000000000000000000, 0.000000000000000000, 1.000000000000000000 ) ) ;
#2683 = DIRECTION ( 'NONE',  ( -1.000000000000000000, 0.000000000000000000, 0.000000000000000000 ) ) ;
#2684 = EDGE_CURVE ( 'NONE', #16829, #4459, #976, .T. ) ;
#2685 = DIRECTION ( 'NONE',  ( 0.000000000000000000, -1.000000000000000000, 0.000000000000000000 ) ) ;
#2686 = CARTESIAN_POINT ( 'NONE',  ( 14.79227890392045452, -2.568991289487080554, -9.169086800441903051 ) ) ;
#2687 = FACE_OUTER_BOUND ( 'NONE', #7204, .T. ) ;
#2688 = EDGE_CURVE ( 'NONE', #886, #2809, #9398, .T. ) ;
#2689 = DIRECTION ( 'NONE',  ( 0.000000000000000000, 0.000000000000000000, -1.000000000000000000 ) ) ;
#2690 = EDGE_CURVE ( 'NONE', #16784, #16942, #13922, .T. ) ;
#2691 = FACE_BOUND ( 'NONE', #19838, .T. ) ;
#2692 = ORIENTED_EDGE ( 'NONE', *, *, #4579, .F. ) ;
#2693 = CARTESIAN_POINT ( 'NONE',  ( 0.000000000000000000, -45.00000000000000000, -23.99999999999999645 ) ) ;
#2694 = ORIENTED_EDGE ( 'NONE', *, *, #16587, .T. ) ;
#2695 = CARTESIAN_POINT ( 'NONE',  ( 74.87477361290781630, 6.123233995736675563E-16, -5.000000000000007994 ) ) ;
#2696 = CARTESIAN_POINT ( 'NONE',  ( -9.363437198784961168, -0.7753088219917839696, 12.13656280121503883 ) ) ;
#2697 = CARTESIAN_POINT ( 'NONE',  ( -9.500000000000000000, -6.482511860946779655E-13, 11.05958914175814556 ) ) ;
#2698 = DIRECTION ( 'NONE',  ( -0.000000000000000000, -0.000000000000000000, -1.000000000000000000 ) ) ;
#2699 = LINE ( 'NONE', #19676, #17937 ) ;
#2700 = ORIENTED_EDGE ( 'NONE', *, *, #18212, .F. ) ;
#2701 = AXIS2_PLACEMENT_3D ( 'NONE', #15454, #19381, #6194 ) ;
#2702 = CARTESIAN_POINT ( 'NONE',  ( -5.871322893124554021, 8.081182679343978492, -7.906742014460233392 ) ) ;
#2703 = CARTESIAN_POINT ( 'NONE',  ( 89.12522638709219791, 7.562528597612068045E-15, 0.000000000000000000 ) ) ;
#2704 = ORIENTED_EDGE ( 'NONE', *, *, #2638, .T. ) ;
#2705 = CARTESIAN_POINT ( 'NONE',  ( -9.500000000000211386, 3.086737114211961064, -8.106742014460232681 ) ) ;
#2706 = ORIENTED_EDGE ( 'NONE', *, *, #16875, .F. ) ;
#2707 = DIRECTION ( 'NONE',  ( -0.000000000000000000, -0.000000000000000000, -1.000000000000000000 ) ) ;
#2708 = CARTESIAN_POINT ( 'NONE',  ( -8.680847955710813579, -2.820578480814257549, 9.733165578109186811 ) ) ;
#2709 = EDGE_CURVE ( 'NONE', #15558, #6547, #2533, .T. ) ;
#2710 = CARTESIAN_POINT ( 'NONE',  ( 77.78386452199872281, 7.420530141404717394E-15, 0.000000000000000000 ) ) ;
#2711 = FACE_OUTER_BOUND ( 'NONE', #15416, .T. ) ;
#2712 = DIRECTION ( 'NONE',  ( -1.000000000000000000, 0.000000000000000000, 0.000000000000000000 ) ) ;
#2713 = AXIS2_PLACEMENT_3D ( 'NONE', #4843, #4479, #12255 ) ;
#2714 = ADVANCED_FACE ( 'NONE', ( #21100 ), #4407, .T. ) ;
#2715 = ORIENTED_EDGE ( 'NONE', *, *, #7071, .T. ) ;
#2716 = ORIENTED_EDGE ( 'NONE', *, *, #12322, .F. ) ;
#2717 = CARTESIAN_POINT ( 'NONE',  ( -35.99999999999995026, 59.99999999999998579, 12.50000000000000000 ) ) ;
#2718 = CONICAL_SURFACE ( 'NONE', #8514, 2.000000000000000000, 0.7853981633974501664 ) ;
#2719 = CARTESIAN_POINT ( 'NONE',  ( -2.935661446561384391, -9.035036904804158553, -10.60674201446023446 ) ) ;
#2720 = ORIENTED_EDGE ( 'NONE', *, *, #19934, .F. ) ;
#2721 = ORIENTED_EDGE ( 'NONE', *, *, #2994, .T. ) ;
#2722 = VECTOR ( 'NONE', #11586, 1000.000000000000000 ) ;
#2723 = DIRECTION ( 'NONE',  ( 1.000000000000000000, 0.000000000000000000, -0.000000000000000000 ) ) ;
#2724 = ORIENTED_EDGE ( 'NONE', *, *, #16561, .T. ) ;
#2725 = DIRECTION ( 'NONE',  ( 1.000000000000000000, 0.000000000000000000, 0.000000000000000000 ) ) ;
#2726 = ORIENTED_EDGE ( 'NONE', *, *, #9425, .T. ) ;
#2727 = DIRECTION ( 'NONE',  ( -0.000000000000000000, -0.000000000000000000, -1.000000000000000000 ) ) ;
#2728 = CARTESIAN_POINT ( 'NONE',  ( 23.00000000000000000, 8.890849273385706297, -7.584660931657394300 ) ) ;
#2729 = CYLINDRICAL_SURFACE ( 'NONE', #7901, 9.500000000000000000 ) ;
#2730 = EDGE_LOOP ( 'NONE', ( #3502, #6520, #7114, #1979 ) ) ;
#2731 = DIRECTION ( 'NONE',  ( 0.8660254037844385966, 0.5000000000000003331, -0.000000000000000000 ) ) ;
#2732 = FACE_OUTER_BOUND ( 'NONE', #10881, .T. ) ;
#2733 = CYLINDRICAL_SURFACE ( 'NONE', #1026, 5.000000000000000888 ) ;
#2734 = ORIENTED_EDGE ( 'NONE', *, *, #10546, .F. ) ;
#2735 = ORIENTED_EDGE ( 'NONE', *, *, #11602, .T. ) ;
#2736 = CARTESIAN_POINT ( 'NONE',  ( 7.685661446561619314, 5.583959896779020049, 6.259589141758143960 ) ) ;
#2737 = ORIENTED_EDGE ( 'NONE', *, *, #8581, .T. ) ;
#2738 = EDGE_CURVE ( 'NONE', #2772, #6705, #12259, .T. ) ;
#2739 = VERTEX_POINT ( 'NONE', #11816 ) ;
#2740 = EDGE_CURVE ( 'NONE', #4272, #18394, #15362, .T. ) ;
#2741 = VERTEX_POINT ( 'NONE', #11341 ) ;
#2742 = EDGE_LOOP ( 'NONE', ( #14466, #22632, #9331, #5030 ) ) ;
#2743 = CARTESIAN_POINT ( 'NONE',  ( -30.16774287754690675, -40.66994976491903913, -1.500000000000000000 ) ) ;
#2744 = CARTESIAN_POINT ( 'NONE',  ( 5.365059087799946447, -7.384370330706356178, -4.333165578109189120 ) ) ;
#2745 = CARTESIAN_POINT ( 'NONE',  ( 0.000000000000000000, 15.03999999999999915, 25.00000000000000000 ) ) ;
#2746 = FACE_OUTER_BOUND ( 'NONE', #22864, .T. ) ;
#2747 = ORIENTED_EDGE ( 'NONE', *, *, #16877, .T. ) ;
#2748 = CARTESIAN_POINT ( 'NONE',  ( -17.15849686392983386, -8.309918483244988607, -4.628645577532794597 ) ) ;
#2749 = CARTESIAN_POINT ( 'NONE',  ( 18.50000000000000000, 15.23000000000000398, -27.00000000000000000 ) ) ;
#2750 = DIRECTION ( 'NONE',  ( 0.000000000000000000, -1.000000000000000000, 0.000000000000000000 ) ) ;
#2751 = ORIENTED_EDGE ( 'NONE', *, *, #2065, .F. ) ;
#2752 = CYLINDRICAL_SURFACE ( 'NONE', #6471, 11.68650000001168721 ) ;
#2753 = DIRECTION ( 'NONE',  ( -1.000000000000000000, 0.000000000000000000, 0.000000000000000000 ) ) ;
#2754 = EDGE_LOOP ( 'NONE', ( #7073, #13249, #11196, #17218, #7090, #9923 ) ) ;
#2755 = CARTESIAN_POINT ( 'NONE',  ( 2.454813078130514813E-15, 16.67999999999999972, 14.50000000000000000 ) ) ;
#2756 = CARTESIAN_POINT ( 'NONE',  ( -14.99999999999999822, -6.045577542124163753E-21, 9.499999999999994671 ) ) ;
#2757 = EDGE_CURVE ( 'NONE', #16379, #11259, #7580, .T. ) ;
#2758 = FACE_OUTER_BOUND ( 'NONE', #22913, .T. ) ;
#2759 = CARTESIAN_POINT ( 'NONE',  ( -5.365059087798940141, -7.384370330707086261, -9.933165578109189653 ) ) ;
#2760 = ORIENTED_EDGE ( 'NONE', *, *, #18947, .F. ) ;
#2761 = EDGE_CURVE ( 'NONE', #6272, #20027, #9911, .T. ) ;
#2762 = DIRECTION ( 'NONE',  ( 0.000000000000000000, -1.000000000000000000, 0.000000000000000000 ) ) ;
#2763 = ORIENTED_EDGE ( 'NONE', *, *, #9897, .F. ) ;
#2764 = VERTEX_POINT ( 'NONE', #742 ) ;
#2765 = CARTESIAN_POINT ( 'NONE',  ( -2.682529543900285862, 8.255977015246234174, 9.233165578109188587 ) ) ;
#2766 = EDGE_CURVE ( 'NONE', #17283, #22874, #8152, .T. ) ;
#2767 = EDGE_CURVE ( 'NONE', #4844, #10574, #23590, .T. ) ;
#2768 = ADVANCED_FACE ( 'NONE', ( #2687 ), #10103, .F. ) ;
#2769 = ORIENTED_EDGE ( 'NONE', *, *, #5081, .F. ) ;
#2770 = LINE ( 'NONE', #6303, #14744 ) ;
#2771 = AXIS2_PLACEMENT_3D ( 'NONE', #7752, #9456, #6067 ) ;
#2772 = VERTEX_POINT ( 'NONE', #19785 ) ;
#2773 = LINE ( 'NONE', #23163, #23195 ) ;
#2774 = CARTESIAN_POINT ( 'NONE',  ( -9.500000000000000000, -6.482511860946779655E-13, -11.05958914175814556 ) ) ;
#2775 = UNCERTAINTY_MEASURE_WITH_UNIT (LENGTH_MEASURE( 1.000000000000000082E-05 ), #14153, 'distance_accuracy_value', 'NONE');
#2776 = CONICAL_SURFACE ( 'NONE', #22642, 2.024999999999999911, 0.7853981633974743692 ) ;
#2777 = CARTESIAN_POINT ( 'NONE',  ( 8.511897654723208362, -2.099402067127519533, 12.50000000000000000 ) ) ;
#2778 = CARTESIAN_POINT ( 'NONE',  ( 0.000000000000000000, 0.000000000000000000, 15.50000000000000000 ) ) ;
#2779 = VERTEX_POINT ( 'NONE', #21478 ) ;
#2780 = CARTESIAN_POINT ( 'NONE',  ( 40.23082370883260239, 29.49999999999999645, -3.000000000000000000 ) ) ;
#2781 = DIRECTION ( 'NONE',  ( 1.000000000000000000, 0.000000000000000000, 0.000000000000000000 ) ) ;
#2782 = DIRECTION ( 'NONE',  ( -1.000000000000000000, -0.000000000000000000, -0.000000000000000000 ) ) ;
#2783 = VERTEX_POINT ( 'NONE', #1582 ) ;
#2784 = CARTESIAN_POINT ( 'NONE',  ( 60.03431729618309021, 6.123233995736659786E-16, -5.000000000000007994 ) ) ;
#2785 = FACE_OUTER_BOUND ( 'NONE', #16371, .T. ) ;
#2786 = DIRECTION ( 'NONE',  ( -1.000000000000000000, 0.000000000000000000, 0.000000000000000000 ) ) ;
#2787 = EDGE_CURVE ( 'NONE', #2253, #8624, #6871, .T. ) ;
#2788 = VECTOR ( 'NONE', #10640, 1000.000000000000000 ) ;
#2789 = LINE ( 'NONE', #4524, #3292 ) ;
#2790 = VERTEX_POINT ( 'NONE', #4902 ) ;
#2791 = AXIS2_PLACEMENT_3D ( 'NONE', #3801, #18100, #8812 ) ;
#2792 = CARTESIAN_POINT ( 'NONE',  ( 5.871322893123449127, 8.081182679344781405, -11.50674201446023126 ) ) ;
#2793=STYLED_ITEM('',(#24141),#10843);
#2794 = VERTEX_POINT ( 'NONE', #3414 ) ;
#2795 = EDGE_LOOP ( 'NONE', ( #19708, #12776 ) ) ;
#2796 = CARTESIAN_POINT ( 'NONE',  ( -9.500000000000211386, 3.086737114211961064, 4.959589141758145026 ) ) ;
#2797 = CARTESIAN_POINT ( 'NONE',  ( 9.500000000000209610, -3.086737114211962396, 11.10674201446023446 ) ) ;
#2798 = EDGE_CURVE ( 'NONE', #7541, #3277, #9957, .T. ) ;
#2799 = EDGE_LOOP ( 'NONE', ( #9949, #13849, #1733, #16162, #14062 ) ) ;
#2800 = CARTESIAN_POINT ( 'NONE',  ( 40.89823313241237912, 26.41789760203348081, 27.00000000000000000 ) ) ;
#2801 = LINE ( 'NONE', #19284, #24037 ) ;
#2802 = CARTESIAN_POINT ( 'NONE',  ( -7.685661446562381371, 5.583959896777970222, 2.859589141758144493 ) ) ;
#2803 = DIRECTION ( 'NONE',  ( -0.000000000000000000, 0.000000000000000000, 1.000000000000000000 ) ) ;
#2804 = PRESENTATION_LAYER_ASSIGNMENT (  '', '', ( #7081 ) ) ;
#2805 = CARTESIAN_POINT ( 'NONE',  ( 15.00000000000000000, 6.781880092842756171E-15, 9.499999999999987566 ) ) ;
#2806 = PRODUCT_DEFINITION_SHAPE ( 'NONE', 'NONE',  #2599 ) ;
#2807 = ORIENTED_EDGE ( 'NONE', *, *, #7972, .F. ) ;
#2808 = DIRECTION ( 'NONE',  ( 0.5735764363510424957, 0.8191520442889943521, 0.000000000000000000 ) ) ;
#2809 = VERTEX_POINT ( 'NONE', #10830 ) ;
#2810 = CARTESIAN_POINT ( 'NONE',  ( 23.00000000000000000, 2.119223430970166522, 17.74893002550480503 ) ) ;
#2811 = CARTESIAN_POINT ( 'NONE',  ( -1.332035614406995583, -9.022543824230414344, 12.38784953505801667 ) ) ;
#2812 = DIRECTION ( 'NONE',  ( 0.000000000000000000, 0.000000000000000000, -1.000000000000000000 ) ) ;
#2813 = CARTESIAN_POINT ( 'NONE',  ( 9.376681730866069486, -1.188761456322952936, 12.06692573382530931 ) ) ;
#2814 = CARTESIAN_POINT ( 'NONE',  ( 28.27483331787887977, 41.23752903419610760, 12.00000000000000000 ) ) ;
#2815 = EDGE_CURVE ( 'NONE', #8713, #9925, #5707, .T. ) ;
#2816 = ORIENTED_EDGE ( 'NONE', *, *, #8520, .F. ) ;
#2817 = DIRECTION ( 'NONE',  ( -0.000000000000000000, -1.000000000000000000, -0.000000000000000000 ) ) ;
#2818 = EDGE_LOOP ( 'NONE', ( #11861, #3603 ) ) ;
#2819 = CARTESIAN_POINT ( 'NONE',  ( 0.000000000000000000, -45.00000000000000000, -23.99999999999999645 ) ) ;
#2820 = CIRCLE ( 'NONE', #1655, 5.024999999999998579 ) ;
#2821 = ORIENTED_EDGE ( 'NONE', *, *, #23692, .T. ) ;
#2822 = CONICAL_SURFACE ( 'NONE', #11347, 5.000000000000007994, 0.9599310885968855844 ) ;
#2823 = DIRECTION ( 'NONE',  ( -1.000000000000000000, -0.000000000000000000, -0.000000000000000000 ) ) ;
#2824 = CARTESIAN_POINT ( 'NONE',  ( 23.00000000000000000, 11.90821470209324140, 7.758837095328885880 ) ) ;
#2825 = AXIS2_PLACEMENT_3D ( 'NONE', #19395, #2669, #15580 ) ;
#2826 = EDGE_CURVE ( 'NONE', #20997, #13001, #16443, .T. ) ;
#2827 = CONICAL_SURFACE ( 'NONE', #23085, 2.000000000000000000, 0.7853981633974501664 ) ;
#2828 = DIRECTION ( 'NONE',  ( -1.000000000000000000, 0.000000000000000000, 0.000000000000000000 ) ) ;
#2829 = DIRECTION ( 'NONE',  ( -1.000000000000000000, -0.000000000000000000, -0.000000000000000000 ) ) ;
#2830 = ORIENTED_EDGE ( 'NONE', *, *, #9423, .F. ) ;
#2831 = DIRECTION ( 'NONE',  ( -1.000000000000000000, 0.000000000000000000, -0.000000000000000000 ) ) ;
#2832 = CARTESIAN_POINT ( 'NONE',  ( 5.871322893124553133, -8.081182679343980269, -8.906742014460233392 ) ) ;
#2833 = EDGE_LOOP ( 'NONE', ( #16684, #17161, #15626, #13597 ) ) ;
#2834 = VERTEX_POINT ( 'NONE', #23911 ) ;
#2835 = CARTESIAN_POINT ( 'NONE',  ( 23.00000000000000000, 11.58003564732003277, 1.573866785045813899 ) ) ;
#2836 = AXIS2_PLACEMENT_3D ( 'NONE', #966, #19635, #10340 ) ;
#2837 = AXIS2_PLACEMENT_3D ( 'NONE', #13150, #16804, #9612 ) ;
#2838 = ADVANCED_FACE ( 'NONE', ( #23785 ), #3061, .T. ) ;
#2839 = DIRECTION ( 'NONE',  ( -1.000000000000000000, -0.000000000000000000, -0.000000000000000000 ) ) ;
#2840 = AXIS2_PLACEMENT_3D ( 'NONE', #11523, #18993, #2267 ) ;
#2841 = CIRCLE ( 'NONE', #15260, 8.000000000000000000 ) ;
#2842 = CARTESIAN_POINT ( 'NONE',  ( -40.77574956473004875, 27.49633847812775400, 11.00000000000000000 ) ) ;
#2843 = AXIS2_PLACEMENT_3D ( 'NONE', #1467, #20121, #16316 ) ;
#2844 = CIRCLE ( 'NONE', #2451, 5.099999999999996980 ) ;
#2845 = EDGE_CURVE ( 'NONE', #21366, #13748, #18558, .T. ) ;
#2846 = ORIENTED_EDGE ( 'NONE', *, *, #17652, .T. ) ;
#2847 = DIRECTION ( 'NONE',  ( -1.000000000000000000, -0.000000000000000000, 0.000000000000000000 ) ) ;
#2848 = CIRCLE ( 'NONE', #22718, 5.000000000000007994 ) ;
#2849 = DIRECTION ( 'NONE',  ( 0.000000000000000000, 0.000000000000000000, 1.000000000000000000 ) ) ;
#2850 = DIRECTION ( 'NONE',  ( 0.000000000000000000, -1.000000000000000000, 0.000000000000000000 ) ) ;
#2851 = SHAPE_REPRESENTATION ( 'Assembly Lag Sleeve', ( #17768, #11496, #628 ), #4129 ) ;
#2852 = EDGE_CURVE ( 'NONE', #14927, #13793, #18060, .T. ) ;
#2853 = LINE ( 'NONE', #10025, #4504 ) ;
#2854 = ORIENTED_EDGE ( 'NONE', *, *, #22440, .F. ) ;
#2855 = DIRECTION ( 'NONE',  ( 1.000000000000000000, 0.000000000000000000, 0.000000000000000000 ) ) ;
#2856 = DIRECTION ( 'NONE',  ( -1.000000000000000000, 0.000000000000000000, 0.000000000000000000 ) ) ;
#2857 = DIRECTION ( 'NONE',  ( -1.000000000000000000, -0.000000000000000000, -0.000000000000000000 ) ) ;
#2858 = CARTESIAN_POINT ( 'NONE',  ( 7.685661446561619314, 5.583959896779020049, 8.259589141758144848 ) ) ;
#2859 = CONICAL_SURFACE ( 'NONE', #3637, 5.025000000000002132, 0.7853981633974482790 ) ;
#2860 = ORIENTED_EDGE ( 'NONE', *, *, #22614, .T. ) ;
#2861 = AXIS2_PLACEMENT_3D ( 'NONE', #23540, #5098, #14468 ) ;
#2862 = VERTEX_POINT ( 'NONE', #21727 ) ;
#2863 = AXIS2_PLACEMENT_3D ( 'NONE', #17003, #11356, #306 ) ;
#2864 = VECTOR ( 'NONE', #421, 1000.000000000000000 ) ;
#2865 = AXIS2_PLACEMENT_3D ( 'NONE', #9047, #14185, #5053 ) ;
#2866 = ORIENTED_EDGE ( 'NONE', *, *, #16646, .T. ) ;
#2867 = CARTESIAN_POINT ( 'NONE',  ( 0.000000000000000000, 45.00000000000000000, -23.99999999999999645 ) ) ;
#2868 = AXIS2_PLACEMENT_3D ( 'NONE', #7210, #14654, #18440 ) ;
#2869 = DIRECTION ( 'NONE',  ( 0.000000000000000000, -0.7557495743542638200, 0.6548607339452786613 ) ) ;
#2870 = DIRECTION ( 'NONE',  ( 1.000000000000000000, 3.469446951953611822E-15, 0.000000000000000000 ) ) ;
#2871 = ORIENTED_EDGE ( 'NONE', *, *, #13640, .F. ) ;
#2872 = CARTESIAN_POINT ( 'NONE',  ( -28.99999999999999645, -29.50000000000001066, -27.00000000000000000 ) ) ;
#2873 = DIRECTION ( 'NONE',  ( -1.000000000000000000, -0.000000000000000000, -0.000000000000000000 ) ) ;
#2874 = VERTEX_POINT ( 'NONE', #6840 ) ;
#2875 = DIRECTION ( 'NONE',  ( -1.000000000000000000, 0.000000000000000000, 0.000000000000000000 ) ) ;
#2876 = CARTESIAN_POINT ( 'NONE',  ( 29.00000000000000355, -29.50000000000000000, -3.000000000000000000 ) ) ;
#2877 = CARTESIAN_POINT ( 'NONE',  ( 5.871322893123449127, 8.081182679344781405, 5.506742014460233925 ) ) ;
#2878 = VECTOR ( 'NONE', #18767, 1000.000000000000000 ) ;
#2879 = ADVANCED_FACE ( 'NONE', ( #9000 ), #14033, .F. ) ;
#2880 = EDGE_CURVE ( 'NONE', #7495, #18986, #18183, .T. ) ;
#2881 = LINE ( 'NONE', #9803, #2220 ) ;
#2882 = FACE_OUTER_BOUND ( 'NONE', #20162, .T. ) ;
#2883 = AXIS2_PLACEMENT_3D ( 'NONE', #7686, #2092, #5871 ) ;
#2884 = CARTESIAN_POINT ( 'NONE',  ( 16.81886298599061291, -7.518780870797755256, -5.825851398835375505 ) ) ;
#2885 = MANIFOLD_SOLID_BREP ( 'ThdSchPat', #9675 ) ;
#2886 = VECTOR ( 'NONE', #13356, 1000.000000000000000 ) ;
#2887 = CARTESIAN_POINT ( 'NONE',  ( 3.890962118697714531E-15, 15.50000000000000000, 7.700000000000001954 ) ) ;
#2888 = CIRCLE ( 'NONE', #16511, 11.68650000001168543 ) ;
#2889 = CARTESIAN_POINT ( 'NONE',  ( -8.680847955711007202, -5.923547351154968927E-13, -7.633165578109188942 ) ) ;
#2890 = ORIENTED_EDGE ( 'NONE', *, *, #17103, .T. ) ;
#2891 = CIRCLE ( 'NONE', #16514, 5.100000000000000533 ) ;
#2892 = CARTESIAN_POINT ( 'NONE',  ( 0.000000000000000000, 0.000000000000000000, 0.000000000000000000 ) ) ;
#2893 = ORIENTED_EDGE ( 'NONE', *, *, #4035, .T. ) ;
#2894 = ORIENTED_EDGE ( 'NONE', *, *, #23368, .T. ) ;
#2895 = AXIS2_PLACEMENT_3D ( 'NONE', #13771, #10088, #21219 ) ;
#2896 = CARTESIAN_POINT ( 'NONE',  ( 8.680847955711199049, -2.820578480813074496, 6.533165578109188409 ) ) ;
#2897 = ORIENTED_EDGE ( 'NONE', *, *, #21028, .T. ) ;
#2898 = CARTESIAN_POINT ( 'NONE',  ( 664.7818939062877917, 858.9837211537981148, 1368.981724745928204 ) ) ;
#2899 = DIRECTION ( 'NONE',  ( 1.000000000000000000, 0.000000000000000000, 0.000000000000000000 ) ) ;
#2900 = ORIENTED_EDGE ( 'NONE', *, *, #4198, .F. ) ;
#2901 = CARTESIAN_POINT ( 'NONE',  ( -36.00000000000000711, -51.00000000000000711, 12.50000000000000000 ) ) ;
#2902 = AXIS2_PLACEMENT_3D ( 'NONE', #16552, #7286, #14830 ) ;
#2903 = EDGE_CURVE ( 'NONE', #15606, #12988, #4953, .T. ) ;
#2904 = AXIS2_PLACEMENT_3D ( 'NONE', #6971, #10732, #12333 ) ;
#2905 = CARTESIAN_POINT ( 'NONE',  ( -0.3960160581560826509, 8.993383190415354278, 101.9803173862455310 ) ) ;
#2906 = CARTESIAN_POINT ( 'NONE',  ( 8.076302169966853128, -3.241261634297146088, 12.50000000000002665 ) ) ;
#2907 = CARTESIAN_POINT ( 'NONE',  ( -9.500000000000000000, -6.482511860946779655E-13, -6.206742014460234103 ) ) ;
#2908 = CIRCLE ( 'NONE', #23946, 4.172000000000008590 ) ;
#2909 = ORIENTED_EDGE ( 'NONE', *, *, #19459, .F. ) ;
#2910 = CARTESIAN_POINT ( 'NONE',  ( 63.81818181818181301, -4.172000000000000597, 5.616230220889771312E-16 ) ) ;
#2911 = VECTOR ( 'NONE', #20824, 999.9999999999998863 ) ;
#2912 = ADVANCED_FACE ( 'NONE', ( #18190 ), #3645, .F. ) ;
#2913 = DIRECTION ( 'NONE',  ( -6.485355633664481337E-14, 1.000000000000000000, 0.000000000000000000 ) ) ;
#2914 = ADVANCED_FACE ( 'NONE', ( #13143 ), #16605, .F. ) ;
#2915 = DIRECTION ( 'NONE',  ( 1.000000000000000000, 0.000000000000000000, 0.000000000000000000 ) ) ;
#2916 = ORIENTED_EDGE ( 'NONE', *, *, #4230, .T. ) ;
#2917 = CARTESIAN_POINT ( 'NONE',  ( -1.999999999999994449, -45.00000000000000000, -23.99999999999999645 ) ) ;
#2918 = DIRECTION ( 'NONE',  ( 0.000000000000000000, 0.000000000000000000, 1.000000000000000000 ) ) ;
#2919 = CARTESIAN_POINT ( 'NONE',  ( -31.74999999999995737, 6.123233995736767268E-16, -5.000000000000000888 ) ) ;
#2920 = ORIENTED_EDGE ( 'NONE', *, *, #6933, .F. ) ;
#2921 = AXIS2_PLACEMENT_3D ( 'NONE', #4688, #14069, #21517 ) ;
#2922 = EDGE_LOOP ( 'NONE', ( #3108, #17399 ) ) ;
#2923 = VECTOR ( 'NONE', #1992, 1000.000000000000000 ) ;
#2924 = VERTEX_POINT ( 'NONE', #15090 ) ;
#2925 = CARTESIAN_POINT ( 'NONE',  ( 9.499999999999790390, 3.086737114213260025, 6.159589141758145203 ) ) ;
#2926 = CARTESIAN_POINT ( 'NONE',  ( -7.685661446562381371, 5.583959896777970222, 12.00674201446023481 ) ) ;
#2927 = AXIS2_PLACEMENT_3D ( 'NONE', #15073, #20953, #4237 ) ;
#2928 = EDGE_LOOP ( 'NONE', ( #4590, #29 ) ) ;
#2929 = MANIFOLD_SOLID_BREP ( 'Chamfer1', #8111 ) ;
#2930 = AXIS2_PLACEMENT_3D ( 'NONE', #23459, #17962, #18985 ) ;
#2931 = LINE ( 'NONE', #6474, #6063 ) ;
#2932 = FACE_OUTER_BOUND ( 'NONE', #23982, .T. ) ;
#2933 = CARTESIAN_POINT ( 'NONE',  ( -28.27483331787888332, -41.23752903419610050, 11.00000000000000000 ) ) ;
#2934 = AXIS2_PLACEMENT_3D ( 'NONE', #233, #19255, #5829 ) ;
#2935 = AXIS2_PLACEMENT_3D ( 'NONE', #19131, #4513, #19387 ) ;
#2936 = ADVANCED_FACE ( 'NONE', ( #18896, #22554 ), #2176, .T. ) ;
#2937 = CARTESIAN_POINT ( 'NONE',  ( -0.9830802669677229932, 45.00000000000000000, 3.000000000000002665 ) ) ;
#2938 = DIRECTION ( 'NONE',  ( 0.000000000000000000, 0.000000000000000000, -1.000000000000000000 ) ) ;
#2939 = CARTESIAN_POINT ( 'NONE',  ( -31.74999999999995737, 6.123233995736767268E-16, -5.000000000000000888 ) ) ;
#2940 = EDGE_LOOP ( 'NONE', ( #12955, #17330, #17250, #12060 ) ) ;
#2941 = EDGE_CURVE ( 'NONE', #6266, #12561, #14624, .T. ) ;
#2942 = EDGE_CURVE ( 'NONE', #21329, #6647, #23968, .T. ) ;
#2943 = VERTEX_POINT ( 'NONE', #14626 ) ;
#2944 = CARTESIAN_POINT ( 'NONE',  ( -27.89784171216405895, -41.49349862090491570, -3.000000000000000000 ) ) ;
#2945 = DIRECTION ( 'NONE',  ( -0.000000000000000000, -0.000000000000000000, -1.000000000000000000 ) ) ;
#2947 = DIRECTION ( 'NONE',  ( -0.000000000000000000, -0.000000000000000000, 1.000000000000000000 ) ) ;
#2946 = AXIS2_PLACEMENT_3D ( 'NONE', #20778, #13687, #4069 ) ;
#2948 = FILL_AREA_STYLE ('',( #4912 ) ) ;
#2949 = CONICAL_SURFACE ( 'NONE', #6060, 1.999999999999994449, 1.029744258676653201 ) ;
#2950 = CARTESIAN_POINT ( 'NONE',  ( -14.51962751333974389, 3.765689428759031010, 27.00000000000000000 ) ) ;
#2951 = ORIENTED_EDGE ( 'NONE', *, *, #14838, .T. ) ;
#2952 = CIRCLE ( 'NONE', #11933, 1.000000000000000888 ) ;
#2953 = DIRECTION ( 'NONE',  ( 0.000000000000000000, 0.000000000000000000, -1.000000000000000000 ) ) ;
#2954 = ORIENTED_EDGE ( 'NONE', *, *, #11297, .F. ) ;
#2955 = CARTESIAN_POINT ( 'NONE',  ( 0.000000000000000000, -12.99147757894464306, 7.750000000000000000 ) ) ;
#2956 = ORIENTED_EDGE ( 'NONE', *, *, #22654, .F. ) ;
#2957 = DIRECTION ( 'NONE',  ( 0.000000000000000000, 0.000000000000000000, 1.000000000000000000 ) ) ;
#2958 = CARTESIAN_POINT ( 'NONE',  ( 23.00000000000000000, -14.80154252341802312, 10.02147513732818851 ) ) ;
#2959 = CARTESIAN_POINT ( 'NONE',  ( 29.00000000000000355, 29.50000000000000000, 27.00000000000000000 ) ) ;
#2960 = CARTESIAN_POINT ( 'NONE',  ( 29.00000000000000000, -29.50000000000000355, 0.000000000000000000 ) ) ;
#2961 = DIRECTION ( 'NONE',  ( 0.000000000000000000, 0.000000000000000000, 1.000000000000000000 ) ) ;
#2962 =( REPRESENTATION_RELATIONSHIP ('NONE','NONE', #21748, #15290 ) REPRESENTATION_RELATIONSHIP_WITH_TRANSFORMATION ( #15137 )SHAPE_REPRESENTATION_RELATIONSHIP( ) );
#2963 = CARTESIAN_POINT ( 'NONE',  ( 29.00000000000000000, 29.50000000000000355, 0.000000000000000000 ) ) ;
#2964 = CIRCLE ( 'NONE', #5694, 18.49999999999999645 ) ;
#2965 = AXIS2_PLACEMENT_3D ( 'NONE', #8992, #6833, #20132 ) ;
#2966 = CIRCLE ( 'NONE', #22457, 5.000000000000004441 ) ;
#2967 = CARTESIAN_POINT ( 'NONE',  ( 69.63636363636364024, 7.491529369508391930E-15, 0.000000000000000000 ) ) ;
#2968 = AXIS2_PLACEMENT_3D ( 'NONE', #10307, #8840, #19477 ) ;
#2969 = AXIS2_PLACEMENT_3D ( 'NONE', #10762, #16731, #14898 ) ;
#2970 = MANIFOLD_SOLID_BREP ( 'Cut-Extrude1', #1145 ) ;
#2971 = CARTESIAN_POINT ( 'NONE',  ( -5.871322893123450015, -8.081182679344781405, -6.506742014460233925 ) ) ;
#2972 = VERTEX_POINT ( 'NONE', #16796 ) ;
#2973 = ORIENTED_EDGE ( 'NONE', *, *, #23743, .F. ) ;
#2974 = EDGE_CURVE ( 'NONE', #9763, #3076, #7406, .T. ) ;
#2975 = FACE_OUTER_BOUND ( 'NONE', #10293, .T. ) ;
#2976 = VERTEX_POINT ( 'NONE', #14969 ) ;
#2977 = CARTESIAN_POINT ( 'NONE',  ( 67.30704456891035647, -5.000000000000000888, 6.123233995736776143E-16 ) ) ;
#2978 = ORIENTED_EDGE ( 'NONE', *, *, #16991, .F. ) ;
#2979 = DIRECTION ( 'NONE',  ( -0.000000000000000000, -0.000000000000000000, 1.000000000000000000 ) ) ;
#2980 = AXIS2_PLACEMENT_3D ( 'NONE', #16196, #19976, #21698 ) ;
#2981 = DIRECTION ( 'NONE',  ( 0.000000000000000000, -0.000000000000000000, -1.000000000000000000 ) ) ;
#2982 = PLANE ( 'NONE',  #8260 ) ;
#2983 = DIRECTION ( 'NONE',  ( -0.000000000000000000, -0.000000000000000000, -1.000000000000000000 ) ) ;
#2984 = AXIS2_PLACEMENT_3D ( 'NONE', #8958, #7022, #8735 ) ;
#2985 = CIRCLE ( 'NONE', #8818, 23.85000000000000142 ) ;
#2986 = CARTESIAN_POINT ( 'NONE',  ( -20.85000000000000497, 15.03999999999999915, 2.200000000000000178 ) ) ;
#2987 = ORIENTED_EDGE ( 'NONE', *, *, #20243, .T. ) ;
#2988 = CARTESIAN_POINT ( 'NONE',  ( -9.500000000000000000, -6.482511860946779655E-13, -10.20674201446023233 ) ) ;
#2989 = DIRECTION ( 'NONE',  ( -1.000000000000000000, 0.000000000000000000, 0.000000000000000000 ) ) ;
#2990 = CARTESIAN_POINT ( 'NONE',  ( -31.74999999999995737, 0.000000000000000000, 0.000000000000000000 ) ) ;
#2991 = CONICAL_SURFACE ( 'NONE', #22087, 5.000000000000007994, 0.9599310885968855844 ) ;
#2992 = CARTESIAN_POINT ( 'NONE',  ( -9.500000000000211386, 3.086737114211961064, 8.959589141758140585 ) ) ;
#2993 = AXIS2_PLACEMENT_3D ( 'NONE', #14742, #9129, #16575 ) ;
#2994 = EDGE_CURVE ( 'NONE', #12373, #430, #4119, .T. ) ;
#2995 = ORIENTED_EDGE ( 'NONE', *, *, #1132, .F. ) ;
#2996 = EDGE_CURVE ( 'NONE', #19937, #1409, #4627, .T. ) ;
#2997 = ORIENTED_EDGE ( 'NONE', *, *, #6080, .T. ) ;
#2998 = CARTESIAN_POINT ( 'NONE',  ( -20.85000000000000853, -15.03999999999999559, 25.00000000000000000 ) ) ;
#2999 = CIRCLE ( 'NONE', #14666, 4.172000000000008590 ) ;
#3000 = CARTESIAN_POINT ( 'NONE',  ( -39.00000000000000000, 28.80990663662251805, 11.00000000000000000 ) ) ;
#3001 = ADVANCED_FACE ( 'NONE', ( #20856 ), #21207, .F. ) ;
#3002 = CARTESIAN_POINT ( 'NONE',  ( 30.68762588338046982, -45.64284848299539732, 0.000000000000000000 ) ) ;
#3003 = CIRCLE ( 'NONE', #14233, 4.499999999999997335 ) ;
#3004 = CYLINDRICAL_SURFACE ( 'NONE', #18872, 6.050000000006050982 ) ;
#3005 = EDGE_CURVE ( 'NONE', #1523, #5235, #15379, .T. ) ;
#3006 = LINE ( 'NONE', #17765, #11238 ) ;
#3007 = VERTEX_POINT ( 'NONE', #23167 ) ;
#3008 = DIRECTION ( 'NONE',  ( -0.000000000000000000, -0.000000000000000000, -1.000000000000000000 ) ) ;
#3009 = CIRCLE ( 'NONE', #6109, 15.00000000000000000 ) ;
#3010 =( BOUNDED_CURVE ( )  B_SPLINE_CURVE ( 2, ( #23145, #10432, #15931, #1067, #17631, #10541, #23636, #1181, #21317, #13872, #8488 ),
 .UNSPECIFIED., .F., .T. ) 
 B_SPLINE_CURVE_WITH_KNOTS ( ( 3, 2, 2, 2, 2, 3 ),
 ( 0.7000000000000000666, 0.7200000000000000844, 0.7400000000000001021, 0.7600000000000000089, 0.7800000000000000266, 0.8000000000000000444 ),
 .UNSPECIFIED. ) 
 CURVE ( )  GEOMETRIC_REPRESENTATION_ITEM ( )  RATIONAL_B_SPLINE_CURVE ( ( 0.9999999999999997780, 0.9510565162951537532, 1.000000000000000000, 0.9510565162951535312, 1.000000000000000000, 0.9510565162951535312, 1.000000000000000000, 0.9510565162951535312, 1.000000000000000000, 0.9510565162951535312, 1.000000000000000000 ) ) 
 REPRESENTATION_ITEM ( '' )  );
#3011 = CARTESIAN_POINT ( 'NONE',  ( 21.85000000000000497, -16.67999999999999616, 13.00000000000000178 ) ) ;
#3012 = CARTESIAN_POINT ( 'NONE',  ( -9.499999999999790390, -3.086737114213257804, 6.306742014460231971 ) ) ;
#3013 = LINE ( 'NONE', #16171, #21435 ) ;
#3014 = CYLINDRICAL_SURFACE ( 'NONE', #3948, 1.999999999999994449 ) ;
#3015 = CARTESIAN_POINT ( 'NONE',  ( 78.94340820527399671, 7.562528597612068045E-15, 0.000000000000000000 ) ) ;
#3016 = CARTESIAN_POINT ( 'NONE',  ( 15.09475045435787877, -4.494086555308249409, -8.407297576120592808 ) ) ;
#3017 = CARTESIAN_POINT ( 'NONE',  ( 0.000000000000000000, 0.000000000000000000, 12.50000000000000000 ) ) ;
#3018 = CARTESIAN_POINT ( 'NONE',  ( 5.365059087799947335, -7.384370330706356178, -4.333165578109189120 ) ) ;
#3019 = CIRCLE ( 'NONE', #22120, 5.000000000000007994 ) ;
#3020 = ORIENTED_EDGE ( 'NONE', *, *, #10934, .F. ) ;
#3021 = DIRECTION ( 'NONE',  ( 0.000000000000000000, 0.000000000000000000, 1.000000000000000000 ) ) ;
#3022 = VERTEX_POINT ( 'NONE', #2408 ) ;
#3023 = CARTESIAN_POINT ( 'NONE',  ( -8.680847955711200825, 2.820578480813073607, 7.533165578109188409 ) ) ;
#3024 = PRODUCT_DEFINITION_SHAPE ( 'NONE', 'NONE',  #13774 ) ;
#3025 = ORIENTED_EDGE ( 'NONE', *, *, #18761, .T. ) ;
#3026 = DIRECTION ( 'NONE',  ( 0.000000000000000000, 0.5783365841231422610, -0.8157982565958178389 ) ) ;
#3027 = CARTESIAN_POINT ( 'NONE',  ( 69.63636363636364024, -4.172000000000000597, 0.000000000000000000 ) ) ;
#3028 = VERTEX_POINT ( 'NONE', #11553 ) ;
#3029 = VERTEX_POINT ( 'NONE', #9712 ) ;
#3030 = EDGE_CURVE ( 'NONE', #21260, #23989, #462, .T. ) ;
#3031 = DIRECTION ( 'NONE',  ( -0.000000000000000000, -0.000000000000000000, -1.000000000000000000 ) ) ;
#3032 = CARTESIAN_POINT ( 'NONE',  ( -9.499999999999790390, -3.086737114213257804, -7.159589141758144315 ) ) ;
#3033 = UNCERTAINTY_MEASURE_WITH_UNIT (LENGTH_MEASURE( 1.000000000000000082E-05 ), #751, 'distance_accuracy_value', 'NONE');
#3034 = ADVANCED_FACE ( 'NONE', ( #4138 ), #12671, .T. ) ;
#3035 = DIRECTION ( 'NONE',  ( -0.000000000000000000, -0.000000000000000000, 1.000000000000000000 ) ) ;
#3036 = DIRECTION ( 'NONE',  ( 0.8757121056631640421, 0.4828336235133042775, 0.000000000000000000 ) ) ;
#3037 = CARTESIAN_POINT ( 'NONE',  ( 0.000000000000000000, 45.00000000000000000, -3.000000000000000000 ) ) ;
#3038 = DIRECTION ( 'NONE',  ( 0.000000000000000000, 0.000000000000000000, 1.000000000000000000 ) ) ;
#3039 = DIRECTION ( 'NONE',  ( 0.000000000000000000, 0.000000000000000000, 1.000000000000000000 ) ) ;
#3040 = CARTESIAN_POINT ( 'NONE',  ( 40.00000000000000711, 29.50000000000000000, 27.00000000000000000 ) ) ;
#3041 = ORIENTED_EDGE ( 'NONE', *, *, #7196, .F. ) ;
#3042 = DIRECTION ( 'NONE',  ( -0.000000000000000000, 0.000000000000000000, -1.000000000000000000 ) ) ;
#3043 = DIRECTION ( 'NONE',  ( -0.000000000000000000, 0.000000000000000000, 1.000000000000000000 ) ) ;
#3044 = CARTESIAN_POINT ( 'NONE',  ( 87.67068093254673045, 7.562528597612068045E-15, 0.000000000000000000 ) ) ;
#3045 = EDGE_LOOP ( 'NONE', ( #22197, #12783, #17080, #561 ) ) ;
#3046 = CARTESIAN_POINT ( 'NONE',  ( -8.680847955710813579, -2.820578480814258437, -5.733165578109188587 ) ) ;
#3047 = VERTEX_POINT ( 'NONE', #20968 ) ;
#3048 = EDGE_LOOP ( 'NONE', ( #20407, #11966, #17754, #17029 ) ) ;
#3049 = CARTESIAN_POINT ( 'NONE',  ( -2.935661446561384391, -9.035036904804158553, 5.459589141758144137 ) ) ;
#3050 = CARTESIAN_POINT ( 'NONE',  ( -2.935661446561384391, -9.035036904804158553, 4.606742014460233570 ) ) ;
#3051 = VECTOR ( 'NONE', #7490, 1000.000000000000000 ) ;
#3052 = ORIENTED_EDGE ( 'NONE', *, *, #16126, .F. ) ;
#3053 = VECTOR ( 'NONE', #6634, 1000.000000000000227 ) ;
#3054 = DIRECTION ( 'NONE',  ( -1.000000000000000000, 0.000000000000000000, 0.000000000000000000 ) ) ;
#3055 = DIRECTION ( 'NONE',  ( -1.000000000000000000, -4.625929269271481378E-15, 0.000000000000000000 ) ) ;
#3056 = EDGE_CURVE ( 'NONE', #20166, #23530, #16554, .T. ) ;
#3057 = DIRECTION ( 'NONE',  ( -0.000000000000000000, -0.000000000000000000, -1.000000000000000000 ) ) ;
#3058 = DIRECTION ( 'NONE',  ( 0.000000000000000000, -1.000000000000000000, 0.000000000000000000 ) ) ;
#3059 = ADVANCED_FACE ( 'NONE', ( #9830 ), #6043, .F. ) ;
#3060 = CARTESIAN_POINT ( 'NONE',  ( 62.94340820527399671, 7.562528597612068045E-15, 0.000000000000000000 ) ) ;
#3061 = CYLINDRICAL_SURFACE ( 'NONE', #15024, 6.050000000006051870 ) ;
#3062 = LINE ( 'NONE', #6957, #3598 ) ;
#3063 = ORIENTED_EDGE ( 'NONE', *, *, #22143, .F. ) ;
#3064 = CARTESIAN_POINT ( 'NONE',  ( -35.99999999999993605, -60.00000000000000000, 0.000000000000000000 ) ) ;
#3065 = CARTESIAN_POINT ( 'NONE',  ( -7.999999999999992895, 0.000000000000000000, 105.0000000000000000 ) ) ;
#3066 = CIRCLE ( 'NONE', #14735, 18.50000000000000000 ) ;
#3067 = CARTESIAN_POINT ( 'NONE',  ( -9.014529360237583333, 3.062692055659724133, -3.500237789100161923 ) ) ;
#3068 = LINE ( 'NONE', #2814, #20650 ) ;
#3069 = ORIENTED_EDGE ( 'NONE', *, *, #1123, .T. ) ;
#3070 = PLANE ( 'NONE',  #7996 ) ;
#3071 = ORIENTED_EDGE ( 'NONE', *, *, #19413, .F. ) ;
#3072 = EDGE_CURVE ( 'NONE', #14555, #1909, #17340, .T. ) ;
#3073 = LINE ( 'NONE', #20028, #7554 ) ;
#3074 = EDGE_LOOP ( 'NONE', ( #22276, #11982, #20661, #14256, #20693, #9824 ) ) ;
#3075 = CYLINDRICAL_SURFACE ( 'NONE', #12164, 6.050000000006052758 ) ;
#3076 = VERTEX_POINT ( 'NONE', #15197 ) ;
#3077 = CARTESIAN_POINT ( 'NONE',  ( -9.000000000000000000, 0.000000000000000000, 105.0000000000000000 ) ) ;
#3078 = CARTESIAN_POINT ( 'NONE',  ( 10.83999999999999986, -14.99147757894464306, 0.000000000000000000 ) ) ;
#3079 = DIRECTION ( 'NONE',  ( 0.000000000000000000, 0.000000000000000000, 1.000000000000000000 ) ) ;
#3080 = DIRECTION ( 'NONE',  ( -0.000000000000000000, -0.000000000000000000, 1.000000000000000000 ) ) ;
#3081 = EDGE_CURVE ( 'NONE', #5584, #10554, #1715, .T. ) ;
#3082 = CARTESIAN_POINT ( 'NONE',  ( 10.40000000000000036, 6.123233995736767268E-16, -5.000000000000000888 ) ) ;
#3083 = EDGE_CURVE ( 'NONE', #14991, #3419, #6199, .T. ) ;
#3084 = EDGE_LOOP ( 'NONE', ( #18596, #12114, #22270, #8230 ) ) ;
#3085 = CARTESIAN_POINT ( 'NONE',  ( 0.000000000000000000, 0.000000000000000000, 0.000000000000000000 ) ) ;
#3086 = CARTESIAN_POINT ( 'NONE',  ( -9.499999999999790390, -3.086737114213257804, -6.306742014460231971 ) ) ;
#3087 = ORIENTED_EDGE ( 'NONE', *, *, #16336, .T. ) ;
#3088 = DIRECTION ( 'NONE',  ( 0.8757121056631640421, -0.4828336235133042775, 0.000000000000000000 ) ) ;
#3089 = DIRECTION ( 'NONE',  ( -1.000000000000000000, -0.000000000000000000, -0.000000000000000000 ) ) ;
#3090 = VERTEX_POINT ( 'NONE', #9960 ) ;
#3091 = DIRECTION ( 'NONE',  ( 0.000000000000000000, 1.000000000000000000, 0.000000000000000000 ) ) ;
#3092 = CARTESIAN_POINT ( 'NONE',  ( 83.30704456891035647, -5.000000000000000888, 6.123233995736776143E-16 ) ) ;
#3093 = EDGE_CURVE ( 'NONE', #12041, #15398, #18521, .T. ) ;
#3094 = DIRECTION ( 'NONE',  ( -1.000000000000000000, 0.000000000000000000, 0.000000000000000000 ) ) ;
#3095 = ORIENTED_EDGE ( 'NONE', *, *, #14707, .F. ) ;
#3096 = APPLICATION_CONTEXT ( 'automotive_design' ) ;
#3097 = CARTESIAN_POINT ( 'NONE',  ( -6.822232771736904647E-13, 9.988891130263535700, -9.706742014460232326 ) ) ;
#3098 = CYLINDRICAL_SURFACE ( 'NONE', #885, 20.85000000000000497 ) ;
#3099 = CARTESIAN_POINT ( 'NONE',  ( -2.935661446562617183, 9.035036904803758873, -4.659589141758143427 ) ) ;
#3100 = CARTESIAN_POINT ( 'NONE',  ( -9.500000000000000000, 1.163414459189985485E-15, -12.00000000000000000 ) ) ;
#3101 = EDGE_LOOP ( 'NONE', ( #17105, #17595, #1143, #7292 ) ) ;
#3102 = ADVANCED_FACE ( 'NONE', ( #17533 ), #8129, .F. ) ;
#3104 = ORIENTED_EDGE ( 'NONE', *, *, #21598, .F. ) ;
#3103 = CIRCLE ( 'NONE', #19484, 1.999999999999994449 ) ;
#3105 = ORIENTED_EDGE ( 'NONE', *, *, #12078, .T. ) ;
#3106 = FACE_OUTER_BOUND ( 'NONE', #13307, .T. ) ;
#3107 = FACE_OUTER_BOUND ( 'NONE', #10013, .T. ) ;
#3108 = ORIENTED_EDGE ( 'NONE', *, *, #20780, .F. ) ;
#3109 = CARTESIAN_POINT ( 'NONE',  ( 0.000000000000000000, -45.00000000000000000, -27.00000000000000000 ) ) ;
#3110 = DIRECTION ( 'NONE',  ( -4.625929269271503466E-15, -1.000000000000000000, 0.000000000000000000 ) ) ;
#3111 = ORIENTED_EDGE ( 'NONE', *, *, #19990, .F. ) ;
#3112 = CARTESIAN_POINT ( 'NONE',  ( -9.999999999999998224, 0.000000000000000000, 15.50000000000000000 ) ) ;
#3113 = CARTESIAN_POINT ( 'NONE',  ( 0.000000000000000000, 0.000000000000000000, 0.000000000000000000 ) ) ;
#3114 = CARTESIAN_POINT ( 'NONE',  ( -5.871322893123450015, -8.081182679344781405, 6.506742014460233925 ) ) ;
#3115 = ADVANCED_FACE ( 'NONE', ( #959 ), #14349, .F. ) ;
#3116 = VERTEX_POINT ( 'NONE', #2907 ) ;
#3117 = DIRECTION ( 'NONE',  ( -0.000000000000000000, -0.000000000000000000, 1.000000000000000000 ) ) ;
#3118 = DIRECTION ( 'NONE',  ( 0.000000000000000000, 1.000000000000000000, 0.000000000000000000 ) ) ;
#3119 = CARTESIAN_POINT ( 'NONE',  ( 17.05196227081077254, -8.053793831531459446, -5.044162359773890714 ) ) ;
#3120 = AXIS2_PLACEMENT_3D ( 'NONE', #10728, #12547, #3536 ) ;
#3121 = DIRECTION ( 'NONE',  ( -1.000000000000000000, -1.224606353822377258E-16, -0.000000000000000000 ) ) ;
#3122 = EDGE_CURVE ( 'NONE', #4244, #19649, #1397, .T. ) ;
#3123 = DIRECTION ( 'NONE',  ( 0.000000000000000000, 0.000000000000000000, 1.000000000000000000 ) ) ;
#3124 = VERTEX_POINT ( 'NONE', #10560 ) ;
#3125 = CARTESIAN_POINT ( 'NONE',  ( 39.99999999999999289, 27.79189783386526358, -27.00000000000000000 ) ) ;
#3126 = VERTEX_POINT ( 'NONE', #5090 ) ;
#3127 = EDGE_CURVE ( 'NONE', #21315, #9633, #20767, .T. ) ;
#3128 = CARTESIAN_POINT ( 'NONE',  ( 8.680847955710813579, 2.820578480814259326, 6.733165578109187699 ) ) ;
#3129 = EDGE_CURVE ( 'NONE', #13291, #10256, #7974, .T. ) ;
#3130 = CARTESIAN_POINT ( 'NONE',  ( 738.2818939062880190, 888.4837211537976600, 1320.481724745927750 ) ) ;
#3131 = DIRECTION ( 'NONE',  ( 1.000000000000000000, -0.000000000000000000, -0.000000000000000000 ) ) ;
#3132 = EDGE_LOOP ( 'NONE', ( #20937, #14012, #9678, #21947, #2227, #6144 ) ) ;
#3133 = CYLINDRICAL_SURFACE ( 'NONE', #3317, 5.000000000000004441 ) ;
#3134 = CARTESIAN_POINT ( 'NONE',  ( -9.500000000000000000, -6.482511860946779655E-13, -9.059589141758143782 ) ) ;
#3135 = AXIS2_PLACEMENT_3D ( 'NONE', #23219, #3513, #23892 ) ;
#3136 = DIRECTION ( 'NONE',  ( -1.000000000000000000, -0.000000000000000000, -0.000000000000000000 ) ) ;
#3137 = DIRECTION ( 'NONE',  ( -1.000000000000000000, -0.000000000000000000, -0.000000000000000000 ) ) ;
#3138 = LINE ( 'NONE', #23299, #16952 ) ;
#3139 = DIRECTION ( 'NONE',  ( -0.000000000000000000, -0.000000000000000000, -1.000000000000000000 ) ) ;
#3140 = EDGE_LOOP ( 'NONE', ( #23236, #15420, #21623, #6765 ) ) ;
#3141 = DIRECTION ( 'NONE',  ( -0.000000000000000000, 1.000000000000000000, 0.000000000000000000 ) ) ;
#3142 = CARTESIAN_POINT ( 'NONE',  ( 67.30704456891035647, 5.000000000000015099, 0.000000000000000000 ) ) ;
#3143 = ADVANCED_FACE ( 'NONE', ( #15950 ), #23529, .F. ) ;
#3144 = CYLINDRICAL_SURFACE ( 'NONE', #18011, 20.85000000000000142 ) ;
#3145 = CARTESIAN_POINT ( 'NONE',  ( 33.25000000000000000, -29.50000000000000000, 12.50000000000000000 ) ) ;
#3146 = DIRECTION ( 'NONE',  ( 0.000000000000000000, -1.000000000000000000, 0.000000000000000000 ) ) ;
#3147 = CARTESIAN_POINT ( 'NONE',  ( 17.59041996266972774, 9.500503876990125107, -0.4759723220310729253 ) ) ;
#3148 = DIRECTION ( 'NONE',  ( -1.000000000000000000, -0.000000000000000000, -0.000000000000000000 ) ) ;
#3149 = ADVANCED_FACE ( 'NONE', ( #14460, #3258 ), #21924, .T. ) ;
#3150 = VERTEX_POINT ( 'NONE', #12149 ) ;
#3151 = CARTESIAN_POINT ( 'NONE',  ( -24.75000000000000000, -29.50000000000000000, -3.000000000000000000 ) ) ;
#3152 = CARTESIAN_POINT ( 'NONE',  ( 7.685661446561619314, 5.583959896779020049, -9.406742014460235168 ) ) ;
#3153 = ORIENTED_EDGE ( 'NONE', *, *, #7078, .F. ) ;
#3154 = EDGE_CURVE ( 'NONE', #7449, #5584, #3138, .T. ) ;
#3155 = ORIENTED_EDGE ( 'NONE', *, *, #10365, .T. ) ;
#3156 = CIRCLE ( 'NONE', #12892, 39.49999999999999289 ) ;
#3157 = CARTESIAN_POINT ( 'NONE',  ( 9.500000000000209610, -3.086737114211962396, 5.959589141758143249 ) ) ;
#3158 = CARTESIAN_POINT ( 'NONE',  ( 9.500000000000000000, 6.470877716354879437E-13, 5.206742014460234103 ) ) ;
#3159 = ORIENTED_EDGE ( 'NONE', *, *, #3474, .T. ) ;
#3160 = DIRECTION ( 'NONE',  ( 1.000000000000000444, -7.999483790236512386E-32, -8.033660851157631600E-27 ) ) ;
#3161 = CARTESIAN_POINT ( 'NONE',  ( -31.74999999999995737, 0.000000000000000000, 0.000000000000000000 ) ) ;
#3162 = DIRECTION ( 'NONE',  ( 0.000000000000000000, 0.000000000000000000, -1.000000000000000000 ) ) ;
#3163 = LINE ( 'NONE', #2939, #16054 ) ;
#3164 = CARTESIAN_POINT ( 'NONE',  ( 23.85000000000000497, 15.03999999999999915, -25.00000000000000000 ) ) ;
#3165 = VERTEX_POINT ( 'NONE', #18157 ) ;
#3166 = COLOUR_RGB ( '',0.7921568627450980005, 0.8196078431372548767, 0.9333333333333333481 ) ;
#3167 = EDGE_LOOP ( 'NONE', ( #17551, #6439, #16128, #23450 ) ) ;
#3168 = CARTESIAN_POINT ( 'NONE',  ( 0.000000000000000000, -15.03999999999999737, 0.000000000000000000 ) ) ;
#3169 = FACE_OUTER_BOUND ( 'NONE', #6961, .T. ) ;
#3170 = AXIS2_PLACEMENT_3D ( 'NONE', #2022, #9446, #22426 ) ;
#3171 = CARTESIAN_POINT ( 'NONE',  ( -4.754193646886300861, 8.248659687480364155, -3.499363352907163272 ) ) ;
#3172 = FACE_OUTER_BOUND ( 'NONE', #20099, .T. ) ;
#3173 = CARTESIAN_POINT ( 'NONE',  ( 20.85000000000000497, 15.03999999999999737, 2.200000000000000178 ) ) ;
#3174 = ADVANCED_FACE ( 'NONE', ( #16197 ), #16303, .F. ) ;
#3175 = EDGE_CURVE ( 'NONE', #3699, #12983, #1455, .T. ) ;
#3176 = FACE_OUTER_BOUND ( 'NONE', #9364, .T. ) ;
#3177 = ORIENTED_EDGE ( 'NONE', *, *, #10395, .T. ) ;
#3178 = DIRECTION ( 'NONE',  ( -1.000000000000000000, -1.224606353822377258E-16, -0.000000000000000000 ) ) ;
#3179 = ORIENTED_EDGE ( 'NONE', *, *, #17629, .F. ) ;
#3180 = DIRECTION ( 'NONE',  ( -0.7071067811865660024, 0.000000000000000000, -0.7071067811865291430 ) ) ;
#3181 = ORIENTED_EDGE ( 'NONE', *, *, #5669, .T. ) ;
#3182 = DIRECTION ( 'NONE',  ( -0.000000000000000000, -0.000000000000000000, -1.000000000000000000 ) ) ;
#3183 = CARTESIAN_POINT ( 'NONE',  ( -29.00000000000000000, 29.49999999999999645, 12.00000000000000000 ) ) ;
#3184 = CARTESIAN_POINT ( 'NONE',  ( 3.890962118697714531E-15, 15.50000000000000000, 7.700000000000001954 ) ) ;
#3185 = VECTOR ( 'NONE', #2808, 1000.000000000000000 ) ;
#3186 = DIRECTION ( 'NONE',  ( 0.000000000000000000, 0.000000000000000000, -1.000000000000000000 ) ) ;
#3187 = CONICAL_SURFACE ( 'NONE', #5142, 4.172000000000008590, 0.9599310885968742602 ) ;
#3188 = EDGE_LOOP ( 'NONE', ( #2623, #21076, #9048, #17038, #18600 ) ) ;
#3189 = DIRECTION ( 'NONE',  ( 0.000000000000000000, -1.000000000000000000, 0.000000000000000000 ) ) ;
#3190 = DIRECTION ( 'NONE',  ( 0.000000000000000000, 0.000000000000000000, 1.000000000000000000 ) ) ;
#3191 = EDGE_CURVE ( 'NONE', #15261, #4544, #5665, .T. ) ;
#3192 = CARTESIAN_POINT ( 'NONE',  ( 5.871322893124553133, -8.081182679343980269, -4.906742014460232504 ) ) ;
#3193 = ORIENTED_EDGE ( 'NONE', *, *, #2815, .F. ) ;
#3194 = ORIENTED_EDGE ( 'NONE', *, *, #19959, .T. ) ;
#3195 = FACE_OUTER_BOUND ( 'NONE', #13125, .T. ) ;
#3196 = DIRECTION ( 'NONE',  ( -0.000000000000000000, -0.000000000000000000, -1.000000000000000000 ) ) ;
#3197 = LINE ( 'NONE', #17972, #19813 ) ;
#3198 = ADVANCED_FACE ( 'NONE', ( #12640 ), #224, .T. ) ;
#3199 = VECTOR ( 'NONE', #10693, 1000.000000000000000 ) ;
#3200 = AXIS2_PLACEMENT_3D ( 'NONE', #8154, #19050, #8042 ) ;
#3201 = EDGE_CURVE ( 'NONE', #10964, #3333, #6455, .T. ) ;
#3202 = CIRCLE ( 'NONE', #13695, 5.000000000000007994 ) ;
#3203 = EDGE_LOOP ( 'NONE', ( #20408, #13044, #12806 ) ) ;
#3204 = CIRCLE ( 'NONE', #489, 1.000000000000000888 ) ;
#3205 = ADVANCED_FACE ( 'NONE', ( #23413 ), #6688, .T. ) ;
#3206 = PRODUCT_DEFINITION_SHAPE ( 'NONE', 'NONE',  #21247 ) ;
#3207 = DIRECTION ( 'NONE',  ( -0.000000000000000000, -0.000000000000000000, 1.000000000000000000 ) ) ;
#3208 = CIRCLE ( 'NONE', #1662, 5.999999999999998224 ) ;
#3209 = CARTESIAN_POINT ( 'NONE',  ( -31.74999999999995737, 6.123233995736767268E-16, -5.000000000000000888 ) ) ;
#3210 = ORIENTED_EDGE ( 'NONE', *, *, #1614, .F. ) ;
#3211 = CONICAL_SURFACE ( 'NONE', #9408, 4.172000000000008590, 0.9599310885968742602 ) ;
#3212 = CARTESIAN_POINT ( 'NONE',  ( -10.49999999999999822, 1.285879139104720633E-15, 2.499999999999999556 ) ) ;
#3213 = DIRECTION ( 'NONE',  ( 0.000000000000000000, 1.000000000000000000, 0.000000000000000000 ) ) ;
#3214 = CARTESIAN_POINT ( 'NONE',  ( 0.000000000000000000, -4.685197434473820088, 9.540979117872439019E-15 ) ) ;
#3215 = CARTESIAN_POINT ( 'NONE',  ( 5.871322893124553133, -8.081182679343980269, 3.759589141758144404 ) ) ;
#3216 = VERTEX_POINT ( 'NONE', #16063 ) ;
#3217 = AXIS2_PLACEMENT_3D ( 'NONE', #2960, #1137, #4564 ) ;
#3219 = AXIS2_PLACEMENT_3D ( 'NONE', #3422, #5375, #12434 ) ;
#3218 = LINE ( 'NONE', #21888, #13905 ) ;
#3220 = CIRCLE ( 'NONE', #15681, 4.171999999999999709 ) ;
#3221 = AXIS2_PLACEMENT_3D ( 'NONE', #14541, #22008, #5287 ) ;
#3222 = FACE_BOUND ( 'NONE', #15127, .T. ) ;
#3223 = EDGE_CURVE ( 'NONE', #17567, #10236, #6811, .T. ) ;
#3224 = CARTESIAN_POINT ( 'NONE',  ( 23.00000000000000000, 6.242160243097161221, 9.879763041175145588 ) ) ;
#3225 = VERTEX_POINT ( 'NONE', #4990 ) ;
#3226 = VERTEX_POINT ( 'NONE', #12406 ) ;
#3227 = CIRCLE ( 'NONE', #15284, 10.49999999999999822 ) ;
#3228 = DIRECTION ( 'NONE',  ( 0.5735764363510427177, -0.8191520442889941300, 1.003171929053527705E-16 ) ) ;
#3229 = CONICAL_SURFACE ( 'NONE', #9068, 4.172000000000008590, 0.9599310885968742602 ) ;
#3230 = ORIENTED_EDGE ( 'NONE', *, *, #18705, .T. ) ;
#3231 = CARTESIAN_POINT ( 'NONE',  ( 9.500000000000000000, 6.470877716354879437E-13, -9.206742014460234103 ) ) ;
#3232 = CARTESIAN_POINT ( 'NONE',  ( 9.500000000000000000, 6.470877716354879437E-13, 5.206742014460234103 ) ) ;
#3233 = CARTESIAN_POINT ( 'NONE',  ( -6.822232771736903637E-13, 9.988891130263535700, 5.706742014460234103 ) ) ;
#3234 = APPLICATION_CONTEXT ( 'automotive_design' ) ;
#3235 = ADVANCED_FACE ( 'NONE', ( #22062 ), #22416, .F. ) ;
#3236 = LINE ( 'NONE', #9071, #6629 ) ;
#3237 = EDGE_CURVE ( 'NONE', #21962, #21867, #22285, .T. ) ;
#3238 = DIRECTION ( 'NONE',  ( -1.000000000000000000, 0.000000000000000000, 0.000000000000000000 ) ) ;
#3239 = CARTESIAN_POINT ( 'NONE',  ( 15.56475192642548500, -5.220978644676161018, 7.947934502462929096 ) ) ;
#3240 = DIRECTION ( 'NONE',  ( -0.000000000000000000, 0.000000000000000000, -1.000000000000000000 ) ) ;
#3241 = DIRECTION ( 'NONE',  ( 1.000000000000000000, 1.224606353822377258E-16, 0.000000000000000000 ) ) ;
#3242 = AXIS2_PLACEMENT_3D ( 'NONE', #11161, #16910, #22542 ) ;
#3243 = AXIS2_PLACEMENT_3D ( 'NONE', #16638, #9295, #20656 ) ;
#3244 = AXIS2_PLACEMENT_3D ( 'NONE', #17007, #18843, #16751 ) ;
#3245 = CARTESIAN_POINT ( 'NONE',  ( 8.680847955710813579, 2.820578480814259326, 10.73316557810918503 ) ) ;
#3246 = VERTEX_POINT ( 'NONE', #22179 ) ;
#3247 = CIRCLE ( 'NONE', #7906, 2.024999999999999911 ) ;
#3248 = CIRCLE ( 'NONE', #158, 49.99999999999998579 ) ;
#3249 = SHAPE_DEFINITION_REPRESENTATION ( #8643, #852 ) ;
#3250 = DIRECTION ( 'NONE',  ( -1.000000000000000000, -0.000000000000000000, -0.000000000000000000 ) ) ;
#3251 = EDGE_LOOP ( 'NONE', ( #22235, #19669, #15345, #3407, #23577, #21907 ) ) ;
#3252 = ORIENTED_EDGE ( 'NONE', *, *, #21530, .T. ) ;
#3253 = DIRECTION ( 'NONE',  ( 1.000000000000000000, 0.000000000000000000, 0.000000000000000000 ) ) ;
#3254 = CARTESIAN_POINT ( 'NONE',  ( 2.935661446561383503, 9.035036904804158553, -6.459589141758144137 ) ) ;
#3255 = CARTESIAN_POINT ( 'NONE',  ( 0.1940582010532044821, 9.000069240190681441, 102.0002077206765563 ) ) ;
#3257 = AXIS2_PLACEMENT_3D ( 'NONE', #23794, #10485, #14499 ) ;
#3256 = CARTESIAN_POINT ( 'NONE',  ( -40.29291594121673370, 26.62062637246459929, 12.00000000000000000 ) ) ;
#3258 = FACE_BOUND ( 'NONE', #7345, .T. ) ;
#3259 = DIRECTION ( 'NONE',  ( -0.000000000000000000, -0.000000000000000000, -1.000000000000000000 ) ) ;
#3260 = VERTEX_POINT ( 'NONE', #20688 ) ;
#3261 = AXIS2_PLACEMENT_3D ( 'NONE', #2127, #7365, #18610 ) ;
#3262 = CARTESIAN_POINT ( 'NONE',  ( 23.00000000000000000, 0.000000000000000000, 0.000000000000000000 ) ) ;
#3263 = CIRCLE ( 'NONE', #6324, 17.87500000001787726 ) ;
#3264 = AXIS2_PLACEMENT_3D ( 'NONE', #2887, #814, #10317 ) ;
#3265 = ORIENTED_EDGE ( 'NONE', *, *, #14687, .T. ) ;
#3266 = DIRECTION ( 'NONE',  ( -0.000000000000000000, -0.000000000000000000, -1.000000000000000000 ) ) ;
#3267 = ORIENTED_EDGE ( 'NONE', *, *, #5847, .F. ) ;
#3268 = ADVANCED_FACE ( 'NONE', ( #5702, #7152 ), #11262, .T. ) ;
#3269 = FACE_OUTER_BOUND ( 'NONE', #2940, .T. ) ;
#3270 = AXIS2_PLACEMENT_3D ( 'NONE', #20453, #3382, #3741 ) ;
#3271 = DIRECTION ( 'NONE',  ( -0.000000000000000000, -0.000000000000000000, -1.000000000000000000 ) ) ;
#3272 =( NAMED_UNIT ( * ) SI_UNIT ( $, .STERADIAN. ) SOLID_ANGLE_UNIT ( ) );
#3273 = LINE ( 'NONE', #7394, #11839 ) ;
#3274 = ORIENTED_EDGE ( 'NONE', *, *, #4287, .F. ) ;
#3275 = DIRECTION ( 'NONE',  ( -1.000000000000000000, -0.000000000000000000, -0.000000000000000000 ) ) ;
#3276 = ORIENTED_EDGE ( 'NONE', *, *, #2128, .T. ) ;
#3277 = VERTEX_POINT ( 'NONE', #7278 ) ;
#3278 = CARTESIAN_POINT ( 'NONE',  ( 2.935661446561383503, 9.035036904804158553, 6.459589141758144137 ) ) ;
#3279 = CARTESIAN_POINT ( 'NONE',  ( -9.500000000000000000, -6.482511860946779655E-13, 8.206742014460234103 ) ) ;
#3280 = ORIENTED_EDGE ( 'NONE', *, *, #9492, .T. ) ;
#3281 = ORIENTED_EDGE ( 'NONE', *, *, #5953, .T. ) ;
#3282 = SHAPE_REPRESENTATION_RELATIONSHIP ( 'NONE' , 'NONE' ,  #358, #11311 ) ;
#3283 = VECTOR ( 'NONE', #15723, 1000.000000000000000 ) ;
#3284 = DIRECTION ( 'NONE',  ( 1.000000000000000000, 0.000000000000000000, 0.000000000000000000 ) ) ;
#3285 = FACE_OUTER_BOUND ( 'NONE', #13998, .T. ) ;
#3286 = VECTOR ( 'NONE', #19576, 999.9999999999998863 ) ;
#3287 = CARTESIAN_POINT ( 'NONE',  ( -2.935661446561384391, -9.035036904804158553, 3.459589141758144137 ) ) ;
#3288 = DIRECTION ( 'NONE',  ( -1.000000000000000000, -1.224606353822377258E-16, -0.000000000000000000 ) ) ;
#3289 = EDGE_CURVE ( 'NONE', #12524, #5796, #20186, .T. ) ;
#3290 = VECTOR ( 'NONE', #23628, 1000.000000000000000 ) ;
#3291 = AXIS2_PLACEMENT_3D ( 'NONE', #19595, #1286, #12484 ) ;
#3292 = VECTOR ( 'NONE', #8262, 1000.000000000000000 ) ;
#3293 = DIRECTION ( 'NONE',  ( -1.000000000000000000, 0.000000000000000000, 0.000000000000000000 ) ) ;
#3294 = CARTESIAN_POINT ( 'NONE',  ( 80.39795365981946418, 7.562528597612068045E-15, 0.000000000000000000 ) ) ;
#3295 = EDGE_CURVE ( 'NONE', #3309, #18951, #4624, .T. ) ;
#3296 = EDGE_CURVE ( 'NONE', #3703, #1523, #11987, .T. ) ;
#3297 = VERTEX_POINT ( 'NONE', #3857 ) ;
#3298 = EDGE_CURVE ( 'NONE', #13441, #18281, #3610, .T. ) ;
#3299 = FILL_AREA_STYLE ('',( #1119 ) ) ;
#3300 = CARTESIAN_POINT ( 'NONE',  ( -6.283940952339894359, 7.151940571226186094, -3.501042821985360654 ) ) ;
#3301 = CARTESIAN_POINT ( 'NONE',  ( 5.078177448618336420, 0.000000000000000000, 0.000000000000000000 ) ) ;
#3302 = TOROIDAL_SURFACE ( 'NONE', #21222, 10.94716442891539643, 0.2999999999999999334 ) ;
#3303 = AXIS2_PLACEMENT_3D ( 'NONE', #13100, #11244, #13214 ) ;
#3304 = CYLINDRICAL_SURFACE ( 'NONE', #13237, 4.249999999999996447 ) ;
#3305 = EDGE_LOOP ( 'NONE', ( #19442, #23543, #11127, #20709, #1270 ) ) ;
#3306 = CARTESIAN_POINT ( 'NONE',  ( 2.682529543900284974, -8.255977015246234174, -8.233165578109190363 ) ) ;
#3307 = TOROIDAL_SURFACE ( 'NONE', #8362, 5.999999999999999112, 1.000000000000000000 ) ;
#3308 = CARTESIAN_POINT ( 'NONE',  ( 0.000000000000000000, -45.00000000000000000, 26.97499999999999432 ) ) ;
#3309 = VERTEX_POINT ( 'NONE', #3494 ) ;
#3310 = CARTESIAN_POINT ( 'NONE',  ( -9.378401895172221003, -4.713374146359802882E-16, -12.12159810482778788 ) ) ;
#3311 = AXIS2_PLACEMENT_3D ( 'NONE', #23174, #10458, #6457 ) ;
#3312 = EDGE_LOOP ( 'NONE', ( #13669, #19594, #13174 ) ) ;
#3313 = DIRECTION ( 'NONE',  ( 1.000000000000000000, 0.000000000000000000, 0.000000000000000000 ) ) ;
#3314 = FACE_OUTER_BOUND ( 'NONE', #965, .T. ) ;
#3315 = VERTEX_POINT ( 'NONE', #13123 ) ;
#3316 = FACE_BOUND ( 'NONE', #1904, .T. ) ;
#3317 = AXIS2_PLACEMENT_3D ( 'NONE', #23651, #17910, #2656 ) ;
#3318 = LINE ( 'NONE', #7080, #4793 ) ;
#3319 = CARTESIAN_POINT ( 'NONE',  ( 75.45454545454545325, 7.491529369508391930E-15, 0.000000000000000000 ) ) ;
#3320 = CARTESIAN_POINT ( 'NONE',  ( 76.90909090909090651, 7.491529369508391930E-15, 0.000000000000000000 ) ) ;
#3321 = EDGE_CURVE ( 'NONE', #16165, #12835, #313, .T. ) ;
#3322 = CARTESIAN_POINT ( 'NONE',  ( 40.00000000000000000, -29.50000000000000000, 27.00000000000000000 ) ) ;
#3323 = ADVANCED_FACE ( 'NONE', ( #2015 ), #7619, .F. ) ;
#3324 = CIRCLE ( 'NONE', #13844, 11.00000000000001066 ) ;
#3325 = CARTESIAN_POINT ( 'NONE',  ( 9.500000000000209610, -3.086737114211962396, -11.95958914175814591 ) ) ;
#3326 = ORIENTED_EDGE ( 'NONE', *, *, #14060, .F. ) ;
#3327 = VECTOR ( 'NONE', #724, 1000.000000000000000 ) ;
#3328 = ORIENTED_EDGE ( 'NONE', *, *, #11680, .F. ) ;
#3329 = DIRECTION ( 'NONE',  ( 0.000000000000000000, 0.000000000000000000, 1.000000000000000000 ) ) ;
#3330 = CARTESIAN_POINT ( 'NONE',  ( 34.10000000000000142, -29.50000000000000355, 12.00000000000000000 ) ) ;
#3331 = AXIS2_PLACEMENT_3D ( 'NONE', #6853, #14282, #8902 ) ;
#3332 = MECHANICAL_DESIGN_GEOMETRIC_PRESENTATION_REPRESENTATION (  '', ( #601 ), #16184 ) ;
#3333 = VERTEX_POINT ( 'NONE', #1555 ) ;
#3334 = CARTESIAN_POINT ( 'NONE',  ( 30.16774287754692807, 40.66994976491903913, -1.500000000000000000 ) ) ;
#3335 = CARTESIAN_POINT ( 'NONE',  ( 77.48886275072855767, 6.123233995736675563E-16, -5.000000000000007994 ) ) ;
#3336 = ORIENTED_EDGE ( 'NONE', *, *, #9299, .T. ) ;
#3337 = CARTESIAN_POINT ( 'NONE',  ( -2.935661446562617183, 9.035036904803758873, -9.806742014460233747 ) ) ;
#3338 = DIRECTION ( 'NONE',  ( -1.000000000000000000, 0.000000000000000000, 0.000000000000000000 ) ) ;
#3339 = PLANE ( 'NONE',  #13083 ) ;
#3340 = VERTEX_POINT ( 'NONE', #23872 ) ;
#3341 = CARTESIAN_POINT ( 'NONE',  ( 27.99999999999998934, 50.99999999999999289, 0.000000000000000000 ) ) ;
#3342 = CIRCLE ( 'NONE', #7216, 20.85000000000000142 ) ;
#3343 = CIRCLE ( 'NONE', #23616, 4.249999999999996447 ) ;
#3344 = ORIENTED_EDGE ( 'NONE', *, *, #1981, .T. ) ;
#3345 = EDGE_CURVE ( 'NONE', #4241, #21197, #14590, .T. ) ;
#3346 = AXIS2_PLACEMENT_3D ( 'NONE', #10896, #67, #13106 ) ;
#3347 = ORIENTED_EDGE ( 'NONE', *, *, #6348, .T. ) ;
#3348 = EDGE_CURVE ( 'NONE', #16364, #555, #12463, .T. ) ;
#3349 = DIRECTION ( 'NONE',  ( -1.000000000000000000, -1.224606353822377258E-16, -0.000000000000000000 ) ) ;
#3350 = EDGE_CURVE ( 'NONE', #1470, #6327, #6553, .T. ) ;
#3351 = DIRECTION ( 'NONE',  ( -1.000000000000000000, 0.000000000000000000, -0.000000000000000000 ) ) ;
#3352 = CARTESIAN_POINT ( 'NONE',  ( 72.54545454545454675, 4.172000000000015696, 0.000000000000000000 ) ) ;
#3353 = ORIENTED_EDGE ( 'NONE', *, *, #11338, .T. ) ;
#3354 = TOROIDAL_SURFACE ( 'NONE', #22855, 14.42592346043842433, 0.2999999999999999334 ) ;
#3355 = DIRECTION ( 'NONE',  ( -1.000000000000000000, -1.224606353822377258E-16, -0.000000000000000000 ) ) ;
#3356 = ORIENTED_EDGE ( 'NONE', *, *, #7133, .T. ) ;
#3357 = LINE ( 'NONE', #10777, #15718 ) ;
#3359 = CARTESIAN_POINT ( 'NONE',  ( -2.935661446562617183, 9.035036904803758873, 3.806742014460233303 ) ) ;
#3358 = VECTOR ( 'NONE', #17650, 1000.000000000000000 ) ;
#3360 = CYLINDRICAL_SURFACE ( 'NONE', #16723, 1.999999999999994449 ) ;
#3361 = DIRECTION ( 'NONE',  ( 1.000000000000000000, 0.000000000000000000, 0.000000000000000000 ) ) ;
#3362 = CARTESIAN_POINT ( 'NONE',  ( 16.19099482616364227, -6.271157271432196367, 7.149633965064770003 ) ) ;
#3363 = AXIS2_PLACEMENT_3D ( 'NONE', #14489, #21609, #18296 ) ;
#3364 = LINE ( 'NONE', #12493, #16120 ) ;
#3365 = CARTESIAN_POINT ( 'NONE',  ( -8.680847955710813579, -2.820578480814257549, -3.733165578109188587 ) ) ;
#3366 = CARTESIAN_POINT ( 'NONE',  ( 1.999999999999997113, -45.00000000000000000, -2.974999999999996092 ) ) ;
#3367 = VERTEX_POINT ( 'NONE', #1394 ) ;
#3368 = CARTESIAN_POINT ( 'NONE',  ( 6.222797240145152671E-13, -9.127583699786111282, 12.13316557810918717 ) ) ;
#3369 = ADVANCED_FACE ( 'NONE', ( #8681 ), #7221, .T. ) ;
#3370 = VERTEX_POINT ( 'NONE', #21871 ) ;
#3371 = AXIS2_PLACEMENT_3D ( 'NONE', #20903, #17216, #7806 ) ;
#3372 =( NAMED_UNIT ( * ) SI_UNIT ( $, .STERADIAN. ) SOLID_ANGLE_UNIT ( ) );
#3373 = PRODUCT_DEFINITION_FORMATION_WITH_SPECIFIED_SOURCE ( 'ANY', '', #18223, .NOT_KNOWN. ) ;
#3374 = DIRECTION ( 'NONE',  ( -1.000000000000000000, -0.000000000000000000, -0.000000000000000000 ) ) ;
#3375 = ORIENTED_EDGE ( 'NONE', *, *, #4061, .F. ) ;
#3376 = ORIENTED_EDGE ( 'NONE', *, *, #2323, .T. ) ;
#3377 = EDGE_CURVE ( 'NONE', #17524, #11505, #13154, .T. ) ;
#3378 = DIRECTION ( 'NONE',  ( -0.000000000000000000, -0.000000000000000000, 1.000000000000000000 ) ) ;
#3379 = CARTESIAN_POINT ( 'NONE',  ( 5.871322893124553133, -8.081182679343980269, -5.759589141758144848 ) ) ;
#3380 = EDGE_CURVE ( 'NONE', #19452, #5210, #5010, .T. ) ;
#3381 = AXIS2_PLACEMENT_3D ( 'NONE', #15861, #2568, #23323 ) ;
#3382 = DIRECTION ( 'NONE',  ( -1.000000000000000000, 0.000000000000000000, 0.000000000000000000 ) ) ;
#3383 = LINE ( 'NONE', #6928, #4540 ) ;
#3384 = DIRECTION ( 'NONE',  ( 0.000000000000000000, 0.000000000000000000, -1.000000000000000000 ) ) ;
#3385 = DIRECTION ( 'NONE',  ( -0.000000000000000000, -0.000000000000000000, -1.000000000000000000 ) ) ;
#3386 = ORIENTED_EDGE ( 'NONE', *, *, #21532, .T. ) ;
#3387 = DIRECTION ( 'NONE',  ( 0.000000000000000000, 0.000000000000000000, 1.000000000000000000 ) ) ;
#3388 = EDGE_LOOP ( 'NONE', ( #2421, #8561, #15254, #22546 ) ) ;
#3389 = AXIS2_PLACEMENT_3D ( 'NONE', #1379, #9019, #16468 ) ;
#3390 = LINE ( 'NONE', #12879, #16440 ) ;
#3391 = VERTEX_POINT ( 'NONE', #18220 ) ;
#3392 = DIRECTION ( 'NONE',  ( 0.000000000000000000, 0.000000000000000000, 1.000000000000000000 ) ) ;
#3393 = CYLINDRICAL_SURFACE ( 'NONE', #4771, 17.87500000001787726 ) ;
#3394 = CARTESIAN_POINT ( 'NONE',  ( 17.52920230446416738, 9.315347328456299536, -1.925892650121554750 ) ) ;
#3395 = DIRECTION ( 'NONE',  ( -1.000000000000000000, -0.000000000000000000, -0.000000000000000000 ) ) ;
#3396 = CARTESIAN_POINT ( 'NONE',  ( 69.05659179472598908, -4.999999999999989342, 0.000000000000000000 ) ) ;
#3397 = ORIENTED_EDGE ( 'NONE', *, *, #18435, .F. ) ;
#3398 = DIRECTION ( 'NONE',  ( 0.000000000000000000, 0.000000000000000000, -1.000000000000000000 ) ) ;
#3399 = CARTESIAN_POINT ( 'NONE',  ( -20.99999999999999645, -29.49999999999999645, 11.50000000000000000 ) ) ;
#3400 = ORIENTED_EDGE ( 'NONE', *, *, #2001, .T. ) ;
#3401 = ADVANCED_FACE ( 'NONE', ( #23945 ), #1146, .F. ) ;
#3402 = ORIENTED_EDGE ( 'NONE', *, *, #14628, .F. ) ;
#3403 = CARTESIAN_POINT ( 'NONE',  ( 2.935661446562616295, -9.035036904803758873, 8.806742014460233747 ) ) ;
#3404 = CARTESIAN_POINT ( 'NONE',  ( 5.871322893124553133, -8.081182679343980269, 8.906742014460233392 ) ) ;
#3405 = DIRECTION ( 'NONE',  ( -1.000000000000000000, 0.000000000000000000, 0.000000000000000000 ) ) ;
#3406 = ORIENTED_EDGE ( 'NONE', *, *, #24004, .T. ) ;
#3407 = ORIENTED_EDGE ( 'NONE', *, *, #11805, .F. ) ;
#3408 = DIRECTION ( 'NONE',  ( 5.501724186093582121E-16, -1.000000000000000000, -0.000000000000000000 ) ) ;
#3409 = DIRECTION ( 'NONE',  ( -0.000000000000000000, -0.000000000000000000, -1.000000000000000000 ) ) ;
#3410 = CARTESIAN_POINT ( 'NONE',  ( 9.500000000000209610, -3.086737114211962396, -5.106742014460234458 ) ) ;
#3411 = ADVANCED_FACE ( 'NONE', ( #12822 ), #12710, .T. ) ;
#3412 = EDGE_CURVE ( 'NONE', #19649, #4244, #7680, .T. ) ;
#3413 = DIRECTION ( 'NONE',  ( 0.000000000000000000, 0.000000000000000000, 1.000000000000000000 ) ) ;
#3414 = CARTESIAN_POINT ( 'NONE',  ( 78.94340820527399671, 6.123233995736675563E-16, -5.000000000000007994 ) ) ;
#3415 = LINE ( 'NONE', #3526, #7861 ) ;
#3416 = PRODUCT ( 'Pin 4X6', 'Pin 4X6', '', ( #15053 ) ) ;
#3417 = EDGE_LOOP ( 'NONE', ( #18996, #14497, #21570, #23141 ) ) ;
#3418 = DIRECTION ( 'NONE',  ( 1.000000000000000000, 1.224606353822377258E-16, 0.000000000000000000 ) ) ;
#3419 = VERTEX_POINT ( 'NONE', #8970 ) ;
#3420 = FACE_BOUND ( 'NONE', #7408, .T. ) ;
#3421 = CARTESIAN_POINT ( 'NONE',  ( 5.871322893123448239, 8.081182679344781405, 10.35958914175814449 ) ) ;
#3422 = CARTESIAN_POINT ( 'NONE',  ( 83.30704456891035647, 7.562528597612068045E-15, 0.000000000000000000 ) ) ;
#3423 = DIRECTION ( 'NONE',  ( -1.000000000000000000, 0.000000000000000000, 0.000000000000000000 ) ) ;
#3424 = DIRECTION ( 'NONE',  ( 0.000000000000000000, -1.000000000000000000, 0.000000000000000000 ) ) ;
#3425 = VERTEX_POINT ( 'NONE', #20111 ) ;
#3426 = AXIS2_PLACEMENT_3D ( 'NONE', #10404, #3259, #20331 ) ;
#3427 = CARTESIAN_POINT ( 'NONE',  ( -14.51962751333974033, -3.765689428759031010, 27.00000000000000000 ) ) ;
#3428 = ORIENTED_EDGE ( 'NONE', *, *, #3668, .F. ) ;
#3429 = CARTESIAN_POINT ( 'NONE',  ( 2.454813078130514813E-15, -16.67999999999999972, 13.00000000000000178 ) ) ;
#3430 = EDGE_LOOP ( 'NONE', ( #22104, #16123, #16319, #22986 ) ) ;
#3431 = EDGE_CURVE ( 'NONE', #23486, #3340, #9223, .T. ) ;
#3432 = CARTESIAN_POINT ( 'NONE',  ( 89.12522638709219791, 5.000000000000015099, 0.000000000000000000 ) ) ;
#3433 = CARTESIAN_POINT ( 'NONE',  ( 1.999999999999996669, -45.00000000000000000, -3.000000000000000000 ) ) ;
#3434 = ORIENTED_EDGE ( 'NONE', *, *, #13022, .T. ) ;
#3435 = FACE_BOUND ( 'NONE', #14343, .T. ) ;
#3436 = LINE ( 'NONE', #18319, #8661 ) ;
#3437 = CARTESIAN_POINT ( 'NONE',  ( 5.365059087798938364, 7.384370330707087149, -10.93316557810918788 ) ) ;
#3438 = EDGE_CURVE ( 'NONE', #4459, #9207, #9635, .T. ) ;
#3439 = CARTESIAN_POINT ( 'NONE',  ( 79.81818181818181301, -4.172000000000000597, 5.616230220889771312E-16 ) ) ;
#3440 = EDGE_CURVE ( 'NONE', #21048, #11189, #22142, .T. ) ;
#3441 = EDGE_LOOP ( 'NONE', ( #4211, #4386, #3915, #5619 ) ) ;
#3442 = FACE_OUTER_BOUND ( 'NONE', #10710, .T. ) ;
#3443 = CARTESIAN_POINT ( 'NONE',  ( 0.000000000000000000, 11.58003564732003277, 1.573866785045813899 ) ) ;
#3444 = CIRCLE ( 'NONE', #23334, 1.500000000000001332 ) ;
#3445 = CARTESIAN_POINT ( 'NONE',  ( 2.935661446562616295, -9.035036904803758873, -5.659589141758144315 ) ) ;
#3446 = ORIENTED_EDGE ( 'NONE', *, *, #7255, .F. ) ;
#3447 = ORIENTED_EDGE ( 'NONE', *, *, #8924, .T. ) ;
#3448 = DIRECTION ( 'NONE',  ( 0.000000000000000000, 0.000000000000000000, -1.000000000000000000 ) ) ;
#3449 = CARTESIAN_POINT ( 'NONE',  ( 42.00000000000000000, 25.22443390181681622, -1.500000000000000000 ) ) ;
#3450 = CARTESIAN_POINT ( 'NONE',  ( 77.78386452199872281, 7.420530141404717394E-15, 0.000000000000000000 ) ) ;
#3451 =( NAMED_UNIT ( * ) PLANE_ANGLE_UNIT ( ) SI_UNIT ( $, .RADIAN. ) );
#3452 = ORIENTED_EDGE ( 'NONE', *, *, #11949, .F. ) ;
#3453 = VECTOR ( 'NONE', #4865, 1000.000000000000000 ) ;
#3454 = DIRECTION ( 'NONE',  ( -1.000000000000000000, 0.000000000000000000, 0.000000000000000000 ) ) ;
#3455 = CARTESIAN_POINT ( 'NONE',  ( 0.000000000000000000, -17.86986844953242937, 0.4282833139926494059 ) ) ;
#3456 = CARTESIAN_POINT ( 'NONE',  ( 0.000000000000000000, -45.00000000000000000, -3.000000000000000000 ) ) ;
#3457 = ORIENTED_EDGE ( 'NONE', *, *, #22102, .T. ) ;
#3458 = CARTESIAN_POINT ( 'NONE',  ( 9.499999999999790390, 3.086737114213260025, -9.306742014460233747 ) ) ;
#3459 = EDGE_CURVE ( 'NONE', #671, #5218, #17045, .T. ) ;
#3460 = CARTESIAN_POINT ( 'NONE',  ( 9.500000000000000000, 6.470877716354879437E-13, 8.059589141758143782 ) ) ;
#3461 = CARTESIAN_POINT ( 'NONE',  ( -9.000000000000000000, 0.000000000000000000, 15.00000000000000178 ) ) ;
#3462 = DIRECTION ( 'NONE',  ( 0.000000000000000000, 0.000000000000000000, 1.000000000000000000 ) ) ;
#3463 = VERTEX_POINT ( 'NONE', #12763 ) ;
#3464 = ORIENTED_EDGE ( 'NONE', *, *, #8873, .T. ) ;
#3465 = DIRECTION ( 'NONE',  ( 0.5000000000000002220, 0.8660254037844384856, 0.000000000000000000 ) ) ;
#3466 = AXIS2_PLACEMENT_3D ( 'NONE', #13674, #21114, #22847 ) ;
#3467 = CARTESIAN_POINT ( 'NONE',  ( 0.000000000000000000, 0.000000000000000000, 0.9999999999999940048 ) ) ;
#3468 = ORIENTED_EDGE ( 'NONE', *, *, #3431, .T. ) ;
#3469 = LINE ( 'NONE', #19947, #15749 ) ;
#3470 = EDGE_LOOP ( 'NONE', ( #457, #7724, #8218, #16655 ) ) ;
#3471 = CARTESIAN_POINT ( 'NONE',  ( -43.50000000000000711, 25.84341543330624091, 0.000000000000000000 ) ) ;
#3472 = CARTESIAN_POINT ( 'NONE',  ( -9.999999999999998224, 15.50000000000000178, -40.80000000000000426 ) ) ;
#3473 = CARTESIAN_POINT ( 'NONE',  ( -29.00000000000000000, 29.49999999999999645, 11.50000000000000000 ) ) ;
#3474 = EDGE_CURVE ( 'NONE', #16460, #7598, #716, .T. ) ;
#3475 = DIRECTION ( 'NONE',  ( -1.000000000000000000, -1.224606353822377258E-16, -0.000000000000000000 ) ) ;
#3476 = FACE_OUTER_BOUND ( 'NONE', #19992, .T. ) ;
#3477 = CARTESIAN_POINT ( 'NONE',  ( 0.000000000000000000, 0.000000000000000000, 105.0000000000000000 ) ) ;
#3478 = CYLINDRICAL_SURFACE ( 'NONE', #15728, 9.500000000000000000 ) ;
#3479 = EDGE_CURVE ( 'NONE', #6633, #20997, #8083, .T. ) ;
#3480 = DIRECTION ( 'NONE',  ( -1.000000000000000000, 0.000000000000000000, 0.000000000000000000 ) ) ;
#3481 = ADVANCED_FACE ( 'NONE', ( #10562 ), #11035, .F. ) ;
#3482 = CARTESIAN_POINT ( 'NONE',  ( 67.30704456891035647, -5.000000000000000000, 6.123233995736775157E-16 ) ) ;
#3483 = ADVANCED_BREP_SHAPE_REPRESENTATION ( '', ( #19017, #8005 ), #14253 ) ;
#3484 = CARTESIAN_POINT ( 'NONE',  ( 5.365059087799946447, -7.384370330706356178, 8.333165578109190008 ) ) ;
#3485 = ORIENTED_EDGE ( 'NONE', *, *, #1632, .F. ) ;
#3486 = APPLICATION_PROTOCOL_DEFINITION ( 'draft international standard', 'automotive_design', 1998, #3874 ) ;
#3487 = CARTESIAN_POINT ( 'NONE',  ( 0.000000000000000000, 0.000000000000000000, -2.500000000000000000 ) ) ;
#3488 = ORIENTED_EDGE ( 'NONE', *, *, #8278, .F. ) ;
#3489 = ORIENTED_EDGE ( 'NONE', *, *, #8439, .F. ) ;
#3490 = CARTESIAN_POINT ( 'NONE',  ( 82.72727272727273373, -4.172000000000000597, 5.616230220889771312E-16 ) ) ;
#3491 = CARTESIAN_POINT ( 'NONE',  ( 5.871322893123449127, 8.081182679344781405, -8.359589141758144493 ) ) ;
#3492 = CARTESIAN_POINT ( 'NONE',  ( -31.74999999999995737, 0.000000000000000000, 0.000000000000000000 ) ) ;
#3493 = DIRECTION ( 'NONE',  ( 0.000000000000000000, 1.000000000000000000, -1.295896757998780388E-15 ) ) ;
#3494 = CARTESIAN_POINT ( 'NONE',  ( 6.699999999999996625, 1.699310525220102153E-15, -13.72592346138681130 ) ) ;
#3495 = DIRECTION ( 'NONE',  ( 1.000000000000000000, 0.000000000000000000, 0.000000000000000000 ) ) ;
#3496 = CIRCLE ( 'NONE', #6626, 17.87500000001787726 ) ;
#3497 = VERTEX_POINT ( 'NONE', #7384 ) ;
#3498 = DIRECTION ( 'NONE',  ( -0.000000000000000000, -0.000000000000000000, -1.000000000000000000 ) ) ;
#3499 = EDGE_CURVE ( 'NONE', #14835, #14761, #2252, .T. ) ;
#3500 = ORIENTED_EDGE ( 'NONE', *, *, #9756, .F. ) ;
#3501 = VECTOR ( 'NONE', #21182, 1000.000000000000000 ) ;
#3502 = ORIENTED_EDGE ( 'NONE', *, *, #9138, .F. ) ;
#3503 = CARTESIAN_POINT ( 'NONE',  ( 50.00005079999999680, 0.000000000000000000, 9.000000000000000000 ) ) ;
#3504 = DIRECTION ( 'NONE',  ( 1.000000000000000000, 0.000000000000000000, 0.000000000000000000 ) ) ;
#3505 = FACE_OUTER_BOUND ( 'NONE', #22019, .T. ) ;
#3506 = SURFACE_STYLE_USAGE ( .BOTH. , #6940 ) ;
#3507 = ADVANCED_FACE ( 'NONE', ( #16670 ), #19812, .T. ) ;
#3508 = CARTESIAN_POINT ( 'NONE',  ( 23.00000000000000000, 5.985147671565880678, -12.89120389306408754 ) ) ;
#3509 = ADVANCED_FACE ( 'NONE', ( #23873 ), #6950, .T. ) ;
#3510 = CARTESIAN_POINT ( 'NONE',  ( 64.39795365981944997, 6.123233995736675563E-16, -5.000000000000007994 ) ) ;
#3511 = EDGE_CURVE ( 'NONE', #17642, #8062, #17452, .T. ) ;
#3512 = ADVANCED_FACE ( 'NONE', ( #1323 ), #14352, .T. ) ;
#3513 = DIRECTION ( 'NONE',  ( -0.000000000000000000, -0.000000000000000000, 1.000000000000000000 ) ) ;
#3514 = ORIENTED_EDGE ( 'NONE', *, *, #6926, .T. ) ;
#3515 = ORIENTED_EDGE ( 'NONE', *, *, #13642, .T. ) ;
#3516 = CARTESIAN_POINT ( 'NONE',  ( -2.935661446561384391, -9.035036904804158553, 8.606742014460234458 ) ) ;
#3517 = CARTESIAN_POINT ( 'NONE',  ( 9.499999999999790390, 3.086737114213260025, 5.306742014460231971 ) ) ;
#3518 = CARTESIAN_POINT ( 'NONE',  ( -39.00000000000000711, 29.49999999999999645, 12.00000000000000000 ) ) ;
#3519 = ORIENTED_EDGE ( 'NONE', *, *, #12606, .T. ) ;
#3520 = ORIENTED_EDGE ( 'NONE', *, *, #22146, .T. ) ;
#3521 = CARTESIAN_POINT ( 'NONE',  ( -41.99999999999999289, 0.000000000000000000, 0.000000000000000000 ) ) ;
#3522 = CIRCLE ( 'NONE', #12838, 1.500000000000001332 ) ;
#3523 = CARTESIAN_POINT ( 'NONE',  ( 23.00000000000000000, 0.000000000000000000, 0.000000000000000000 ) ) ;
#3524 = CARTESIAN_POINT ( 'NONE',  ( 23.00000000000000000, 0.000000000000000000, 0.000000000000000000 ) ) ;
#3525 = DIRECTION ( 'NONE',  ( -0.000000000000000000, -0.000000000000000000, 1.000000000000000000 ) ) ;
#3526 = CARTESIAN_POINT ( 'NONE',  ( -14.51962751333974033, -3.765689428759031010, 27.00000000000000000 ) ) ;
#3527 = LINE ( 'NONE', #1933, #6711 ) ;
#3528 = EDGE_CURVE ( 'NONE', #23675, #8495, #16285, .T. ) ;
#3529 = ORIENTED_EDGE ( 'NONE', *, *, #5774, .F. ) ;
#3530 = CARTESIAN_POINT ( 'NONE',  ( -40.89823313241237912, 26.41789760203348081, 27.00000000000000000 ) ) ;
#3531 = CARTESIAN_POINT ( 'NONE',  ( 0.000000000000000000, 0.000000000000000000, 0.000000000000000000 ) ) ;
#3532 = CARTESIAN_POINT ( 'NONE',  ( 0.9999999999999986677, 0.000000000000000000, 13.72592346138681130 ) ) ;
#3533 = CARTESIAN_POINT ( 'NONE',  ( -28.99999999999999645, 29.50000000000000711, -1.500000000000000000 ) ) ;
#3534 = DIRECTION ( 'NONE',  ( -0.000000000000000000, -0.000000000000000000, -1.000000000000000000 ) ) ;
#3535 = AXIS2_PLACEMENT_3D ( 'NONE', #16729, #14782, #9385 ) ;
#3536 = DIRECTION ( 'NONE',  ( 0.000000000000000000, -1.000000000000000000, 0.000000000000000000 ) ) ;
#3537 = ADVANCED_FACE ( 'NONE', ( #24000 ), #7328, .T. ) ;
#3538 = EDGE_CURVE ( 'NONE', #13580, #12511, #3444, .T. ) ;
#3539 = DIRECTION ( 'NONE',  ( 0.7071067811865660024, 0.000000000000000000, 0.7071067811865291430 ) ) ;
#3540 = VERTEX_POINT ( 'NONE', #14593 ) ;
#3541 = CARTESIAN_POINT ( 'NONE',  ( 87.67068093254673045, -5.000000000000000888, 6.123233995736776143E-16 ) ) ;
#3542 = ORIENTED_EDGE ( 'NONE', *, *, #15364, .T. ) ;
#3543 = CARTESIAN_POINT ( 'NONE',  ( 6.809999908187194197E-13, -9.988891130263535700, -9.559589141758145558 ) ) ;
#3544 = ORIENTED_EDGE ( 'NONE', *, *, #1730, .F. ) ;
#3545 = DIRECTION ( 'NONE',  ( -1.000000000000000000, -1.224606353822377258E-16, -0.000000000000000000 ) ) ;
#3546 = CARTESIAN_POINT ( 'NONE',  ( 76.03431729618309021, -5.000000000000000000, 6.123233995736775157E-16 ) ) ;
#3547 = AXIS2_PLACEMENT_3D ( 'NONE', #20701, #15316, #7510 ) ;
#3548 = APPLICATION_CONTEXT ( 'automotive_design' ) ;
#3549 = CARTESIAN_POINT ( 'NONE',  ( 6.809999908187194197E-13, -9.988891130263535700, -7.559589141758143782 ) ) ;
#3550 = EDGE_LOOP ( 'NONE', ( #16182, #4664, #18580, #21636 ) ) ;
#3551 = ORIENTED_EDGE ( 'NONE', *, *, #21387, .F. ) ;
#3552 = LINE ( 'NONE', #1612, #6431 ) ;
#3553 = CARTESIAN_POINT ( 'NONE',  ( 62.36363636363636687, 4.172000000000015696, 0.000000000000000000 ) ) ;
#3554 =( LENGTH_UNIT ( ) NAMED_UNIT ( * ) SI_UNIT ( .MILLI., .METRE. ) );
#3555 = ORIENTED_EDGE ( 'NONE', *, *, #17154, .T. ) ;
#3556 = EDGE_CURVE ( 'NONE', #20567, #16706, #22938, .T. ) ;
#3557 = DIRECTION ( 'NONE',  ( -0.000000000000000000, 0.000000000000000000, -1.000000000000000000 ) ) ;
#3558 = DIRECTION ( 'NONE',  ( -0.000000000000000000, -0.000000000000000000, -1.000000000000000000 ) ) ;
#3559 = AXIS2_PLACEMENT_3D ( 'NONE', #18340, #23614, #20183 ) ;
#3560 = EDGE_LOOP ( 'NONE', ( #10483, #5200, #15187, #12381 ) ) ;
#3561 = CARTESIAN_POINT ( 'NONE',  ( -28.00000000000000355, -51.00000000000000711, 0.5000000000000000000 ) ) ;
#3562 = CARTESIAN_POINT ( 'NONE',  ( 5.000000000000000000, 0.000000000000000000, 0.000000000000000000 ) ) ;
#3563 = AXIS2_PLACEMENT_3D ( 'NONE', #9163, #23713, #16486 ) ;
#3564 = CARTESIAN_POINT ( 'NONE',  ( 0.9999999999999986677, 11.22592346138681130, 0.000000000000000000 ) ) ;
#3565 = AXIS2_PLACEMENT_3D ( 'NONE', #3586, #14697, #5185 ) ;
#3566 = CARTESIAN_POINT ( 'NONE',  ( -5.365059087799947335, 7.384370330706355290, 3.333165578109187344 ) ) ;
#3567 = ORIENTED_EDGE ( 'NONE', *, *, #7832, .F. ) ;
#3568 = ORIENTED_EDGE ( 'NONE', *, *, #535, .F. ) ;
#3569 = ORIENTED_EDGE ( 'NONE', *, *, #19604, .F. ) ;
#3570 = ORIENTED_EDGE ( 'NONE', *, *, #13361, .F. ) ;
#3571 = DIRECTION ( 'NONE',  ( -0.000000000000000000, -0.000000000000000000, 1.000000000000000000 ) ) ;
#3572 = EDGE_CURVE ( 'NONE', #18241, #11779, #22158, .T. ) ;
#3573 = DIRECTION ( 'NONE',  ( 0.000000000000000000, 1.000000000000000000, 0.000000000000000000 ) ) ;
#3574 = EDGE_LOOP ( 'NONE', ( #13850, #18168, #6301, #1574 ) ) ;
#3575 = CARTESIAN_POINT ( 'NONE',  ( 0.000000000000000000, -9.239931321968100519, -10.79948145182508057 ) ) ;
#3576 = AXIS2_PLACEMENT_3D ( 'NONE', #11920, #13639, #7653 ) ;
#3577 = EDGE_CURVE ( 'NONE', #21069, #2444, #19035, .T. ) ;
#3578 = AXIS2_PLACEMENT_3D ( 'NONE', #380, #16828, #3912 ) ;
#3579 = DIRECTION ( 'NONE',  ( -0.000000000000000000, -0.000000000000000000, -1.000000000000000000 ) ) ;
#3580 = VECTOR ( 'NONE', #4283, 1000.000000000000000 ) ;
#3581 = ORIENTED_EDGE ( 'NONE', *, *, #6763, .F. ) ;
#3582 = CARTESIAN_POINT ( 'NONE',  ( -29.00000000000000000, -29.49999999999999645, 11.50000000000000000 ) ) ;
#3583 = CARTESIAN_POINT ( 'NONE',  ( 76.32931906745326955, 7.420530141404717394E-15, 0.000000000000000000 ) ) ;
#3584 = EDGE_CURVE ( 'NONE', #15649, #16325, #9268, .T. ) ;
#3585 = FACE_OUTER_BOUND ( 'NONE', #7462, .T. ) ;
#3586 = CARTESIAN_POINT ( 'NONE',  ( 41.00000000000000000, -1.387778780781445676E-14, 8.500000000000000000 ) ) ;
#3587 = DIRECTION ( 'NONE',  ( -0.000000000000000000, -0.000000000000000000, 1.000000000000000000 ) ) ;
#3588 = CARTESIAN_POINT ( 'NONE',  ( 14.80736872429922002, -4.130115634539738068, 8.564444421911355576 ) ) ;
#3589 = DIRECTION ( 'NONE',  ( -1.000000000000000000, 0.000000000000000000, 0.000000000000000000 ) ) ;
#3590 = CARTESIAN_POINT ( 'NONE',  ( 23.00000000000000000, -13.66196005206966468, 3.918670437617043145 ) ) ;
#3591 = CARTESIAN_POINT ( 'NONE',  ( 9.324366623732823450E-16, 111.0000000000000000, 80.99999999999998579 ) ) ;
#3592 = DIRECTION ( 'NONE',  ( 0.000000000000000000, -1.000000000000000000, 9.256405414277000802E-16 ) ) ;
#3593 = ORIENTED_EDGE ( 'NONE', *, *, #42, .F. ) ;
#3594 = ORIENTED_EDGE ( 'NONE', *, *, #23162, .F. ) ;
#3595 = CARTESIAN_POINT ( 'NONE',  ( 8.680847955711199049, -2.820578480813074496, 10.53316557810918752 ) ) ;
#3596 = VERTEX_POINT ( 'NONE', #11263 ) ;
#3597 = AXIS2_PLACEMENT_3D ( 'NONE', #19807, #8174, #23350 ) ;
#3598 = VECTOR ( 'NONE', #17828, 1000.000000000000114 ) ;
#3599 = PRODUCT_CONTEXT ( 'NONE', #5272, 'mechanical' ) ;
#3600 = VECTOR ( 'NONE', #4184, 1000.000000000000000 ) ;
#3601 = CARTESIAN_POINT ( 'NONE',  ( 20.64923905428956630, 37.45138642374539728, 11.00000000000000000 ) ) ;
#3602 = CONICAL_SURFACE ( 'NONE', #22324, 9.000000000000001776, 0.7853981633974431720 ) ;
#3603 = ORIENTED_EDGE ( 'NONE', *, *, #23310, .F. ) ;
#3604 = ORIENTED_EDGE ( 'NONE', *, *, #15079, .F. ) ;
#3605 = CARTESIAN_POINT ( 'NONE',  ( -7.865713094527578164, 5.334608486671521099, -12.00987729971068774 ) ) ;
#3606 = CARTESIAN_POINT ( 'NONE',  ( -6.233975306307046963E-13, 9.127583699786111282, -9.133165578109188942 ) ) ;
#3607 = EDGE_LOOP ( 'NONE', ( #17880, #12437, #22439, #2706 ) ) ;
#3608 = DIRECTION ( 'NONE',  ( -1.000000000000000000, -1.224606353822377258E-16, -0.000000000000000000 ) ) ;
#3609 = LINE ( 'NONE', #18862, #16227 ) ;
#3610 = LINE ( 'NONE', #18508, #3051 ) ;
#3611 = ADVANCED_FACE ( 'NONE', ( #13124 ), #20690, .T. ) ;
#3612 = EDGE_CURVE ( 'NONE', #8536, #7965, #3066, .T. ) ;
#3613 = CARTESIAN_POINT ( 'NONE',  ( 0.000000000000000000, -45.00000000000000000, 3.000000000000002665 ) ) ;
#3614 = CARTESIAN_POINT ( 'NONE',  ( 29.00000000000000000, 29.50000000000000355, 12.00000000000000000 ) ) ;
#3615 = CARTESIAN_POINT ( 'NONE',  ( 44.99999999999998579, -51.00000000000000711, 12.50000000000000000 ) ) ;
#3616 = ORIENTED_EDGE ( 'NONE', *, *, #5515, .T. ) ;
#3617 = VECTOR ( 'NONE', #89, 1000.000000000000000 ) ;
#3618 = TOROIDAL_SURFACE ( 'NONE', #23509, 49.00000000000000000, 1.000000000000000000 ) ;
#3619 = VERTEX_POINT ( 'NONE', #3974 ) ;
#3620 = DIRECTION ( 'NONE',  ( -0.000000000000000000, 1.000000000000000000, 1.224646799147353207E-16 ) ) ;
#3621 = CARTESIAN_POINT ( 'NONE',  ( 84.76159002345582394, 7.562528597612068045E-15, 0.000000000000000000 ) ) ;
#3622 = CARTESIAN_POINT ( 'NONE',  ( 34.10000000000000853, 29.50000000000000000, -27.00000000000000000 ) ) ;
#3623 =( LENGTH_UNIT ( ) NAMED_UNIT ( * ) SI_UNIT ( .MILLI., .METRE. ) );
#3624 = VECTOR ( 'NONE', #22848, 999.9999999999998863 ) ;
#3625 = CIRCLE ( 'NONE', #18437, 1.499999999999999556 ) ;
#3626 = DIRECTION ( 'NONE',  ( 0.8298699724180977899, -0.5579568342432823513, 0.000000000000000000 ) ) ;
#3627 = LINE ( 'NONE', #6943, #10230 ) ;
#3628 = CARTESIAN_POINT ( 'NONE',  ( -9.500000000000211386, 3.086737114211961064, -10.10674201446023446 ) ) ;
#3629 =( BOUNDED_CURVE ( )  B_SPLINE_CURVE ( 2, ( #7497, #22778, #7853, #22648, #6062, #20950, #5928, #1803, #14951, #9228, #5711 ),
 .UNSPECIFIED., .F., .T. ) 
 B_SPLINE_CURVE_WITH_KNOTS ( ( 3, 2, 2, 2, 2, 3 ),
 ( 0.4000000000000000222, 0.4199999999999999845, 0.4400000000000000022, 0.4600000000000000200, 0.4799999999999999822, 0.5000000000000000000 ),
 .UNSPECIFIED. ) 
 CURVE ( )  GEOMETRIC_REPRESENTATION_ITEM ( )  RATIONAL_B_SPLINE_CURVE ( ( 1.000000000000000000, 0.9510565162951535312, 1.000000000000000000, 0.9510565162951535312, 1.000000000000000000, 0.9510565162951535312, 1.000000000000000000, 0.9510565162951535312, 1.000000000000000000, 0.9510565162951535312, 1.000000000000000000 ) ) 
 REPRESENTATION_ITEM ( '' )  );
#3630 = DIRECTION ( 'NONE',  ( -1.000000000000000000, -0.000000000000000000, -0.000000000000000000 ) ) ;
#3631 = ORIENTED_EDGE ( 'NONE', *, *, #16637, .T. ) ;
#3632 = EDGE_LOOP ( 'NONE', ( #7754, #3159, #9317, #18659 ) ) ;
#3633 = CARTESIAN_POINT ( 'NONE',  ( 9.500000000000209610, -3.086737114211962396, 7.106742014460232681 ) ) ;
#3634 = ORIENTED_EDGE ( 'NONE', *, *, #19149, .T. ) ;
#3635 = ORIENTED_EDGE ( 'NONE', *, *, #8061, .F. ) ;
#3636 = EDGE_CURVE ( 'NONE', #13806, #12252, #11525, .T. ) ;
#3637 = AXIS2_PLACEMENT_3D ( 'NONE', #2876, #1295, #10171 ) ;
#3638 = AXIS2_PLACEMENT_3D ( 'NONE', #15712, #12161, #17806 ) ;
#3639 = DIRECTION ( 'NONE',  ( 0.000000000000000000, 0.000000000000000000, 1.000000000000000000 ) ) ;
#3640 = VECTOR ( 'NONE', #9641, 1000.000000000000000 ) ;
#3641 = CIRCLE ( 'NONE', #10252, 5.000000000000007994 ) ;
#3642 = ADVANCED_FACE ( 'NONE', ( #565 ), #18864, .T. ) ;
#3643 = AXIS2_PLACEMENT_3D ( 'NONE', #541, #7961, #13590 ) ;
#3644 = CARTESIAN_POINT ( 'NONE',  ( 35.99999999999999289, -51.00000000000000711, 0.5000000000000000000 ) ) ;
#3645 = PLANE ( 'NONE',  #2993 ) ;
#3646 = CARTESIAN_POINT ( 'NONE',  ( -23.85000000000000497, 15.03999999999999915, 25.00000000000000000 ) ) ;
#3647 = EDGE_CURVE ( 'NONE', #15990, #19865, #327, .T. ) ;
#3648 = EDGE_CURVE ( 'NONE', #5402, #891, #9575, .T. ) ;
#3649 = AXIS2_PLACEMENT_3D ( 'NONE', #15088, #12900, #12789 ) ;
#3650 = CARTESIAN_POINT ( 'NONE',  ( 9.499999999999790390, 3.086737114213260025, -10.15958914175814343 ) ) ;
#3651 = VERTEX_POINT ( 'NONE', #7986 ) ;
#3652 = FACE_OUTER_BOUND ( 'NONE', #16888, .T. ) ;
#3653 = CARTESIAN_POINT ( 'NONE',  ( 66.14750088563508257, 7.420530141404717394E-15, 0.000000000000000000 ) ) ;
#3654 = DIRECTION ( 'NONE',  ( -1.000000000000000000, -0.000000000000000000, -0.000000000000000000 ) ) ;
#3655 = CARTESIAN_POINT ( 'NONE',  ( -36.00000000000000711, -51.00000000000000711, 0.5000000000000000000 ) ) ;
#3656 = CYLINDRICAL_SURFACE ( 'NONE', #11657, 6.050000000006050982 ) ;
#3657 = CARTESIAN_POINT ( 'NONE',  ( 2.682529543899157876, 8.255977015246598327, -9.033165578109187521 ) ) ;
#3658 = CIRCLE ( 'NONE', #5614, 4.172000000000008590 ) ;
#3659 = DIRECTION ( 'NONE',  ( -1.000000000000000000, 0.000000000000000000, 0.000000000000000000 ) ) ;
#3660 = EDGE_LOOP ( 'NONE', ( #549, #11280, #19293, #10654 ) ) ;
#3661 = CIRCLE ( 'NONE', #20029, 5.100000000000000533 ) ;
#3662 = ORIENTED_EDGE ( 'NONE', *, *, #10766, .F. ) ;
#3663 = CARTESIAN_POINT ( 'NONE',  ( -34.10000000000000142, 29.50000000000000000, 27.00000000000000000 ) ) ;
#3664 = AXIS2_PLACEMENT_3D ( 'NONE', #14671, #14417, #21652 ) ;
#3665 = DIRECTION ( 'NONE',  ( -0.000000000000000000, -0.000000000000000000, -1.000000000000000000 ) ) ;
#3666 = CIRCLE ( 'NONE', #1334, 5.000000000000007994 ) ;
#3667 = ORIENTED_EDGE ( 'NONE', *, *, #7536, .T. ) ;
#3668 = EDGE_CURVE ( 'NONE', #4544, #11156, #20980, .T. ) ;
#3669 = EDGE_CURVE ( 'NONE', #5827, #5686, #24085, .T. ) ;
#3670 = CARTESIAN_POINT ( 'NONE',  ( -9.500000000000000000, -6.482511860946779655E-13, -3.059589141758143338 ) ) ;
#3671 = VECTOR ( 'NONE', #17430, 1000.000000000000000 ) ;
#3672 = DIRECTION ( 'NONE',  ( -1.000000000000000000, -1.224606353822377258E-16, -0.000000000000000000 ) ) ;
#3673 = CARTESIAN_POINT ( 'NONE',  ( -20.85000000000000853, -15.03999999999999737, 27.00000000000000000 ) ) ;
#3674 = ADVANCED_FACE ( 'NONE', ( #22641 ), #2271, .F. ) ;
#3675 = EDGE_CURVE ( 'NONE', #14640, #14835, #9440, .T. ) ;
#3676 = EDGE_CURVE ( 'NONE', #9714, #8913, #18995, .T. ) ;
#3677 = VECTOR ( 'NONE', #11162, 1000.000000000000000 ) ;
#3678 = CARTESIAN_POINT ( 'NONE',  ( -6.822232771736903637E-13, 9.988891130263535700, -8.559589141758145558 ) ) ;
#3679 = ORIENTED_EDGE ( 'NONE', *, *, #13363, .T. ) ;
#3680 = VECTOR ( 'NONE', #4028, 1000.000000000000000 ) ;
#3681 = ORIENTED_EDGE ( 'NONE', *, *, #11214, .F. ) ;
#3682 = CARTESIAN_POINT ( 'NONE',  ( 0.000000000000000000, 0.000000000000000000, 15.00000000000000178 ) ) ;
#3683 = ORIENTED_EDGE ( 'NONE', *, *, #15336, .F. ) ;
#3684 = AXIS2_PLACEMENT_3D ( 'NONE', #17884, #10533, #8212 ) ;
#3685 = CARTESIAN_POINT ( 'NONE',  ( 0.000000000000000000, -12.99147757894464306, 6.750000000000000888 ) ) ;
#3686 = AXIS2_PLACEMENT_3D ( 'NONE', #22286, #11390, #5563 ) ;
#3687 = VERTEX_POINT ( 'NONE', #7623 ) ;
#3688 = DIRECTION ( 'NONE',  ( -0.000000000000000000, -0.000000000000000000, -1.000000000000000000 ) ) ;
#3689 = DIRECTION ( 'NONE',  ( -1.000000000000000000, -1.224606353822377258E-16, -0.000000000000000000 ) ) ;
#3690 = ORIENTED_EDGE ( 'NONE', *, *, #23588, .F. ) ;
#3691 = CARTESIAN_POINT ( 'NONE',  ( -42.38288618805137276, -26.96649534593477426, 0.000000000000000000 ) ) ;
#3692 = CARTESIAN_POINT ( 'NONE',  ( 2.024999999999999911, 45.00000000000000000, 27.00000000000000000 ) ) ;
#3693 = CARTESIAN_POINT ( 'NONE',  ( 44.99999999999998579, -51.00000000000000711, 0.000000000000000000 ) ) ;
#3694 = CARTESIAN_POINT ( 'NONE',  ( -41.73082370883257397, -27.62204025492845361, -1.500000000000000000 ) ) ;
#3695 = VECTOR ( 'NONE', #22906, 1000.000000000000000 ) ;
#3696 = AXIS2_PLACEMENT_3D ( 'NONE', #18669, #7201, #16459 ) ;
#3697 = CARTESIAN_POINT ( 'NONE',  ( -7.022953521755574080, 5.102474405759713783, 5.433165578109188765 ) ) ;
#3698 = ORIENTED_EDGE ( 'NONE', *, *, #834, .F. ) ;
#3699 = VERTEX_POINT ( 'NONE', #328 ) ;
#3700 = VECTOR ( 'NONE', #22783, 1000.000000000000000 ) ;
#3701 = ORIENTED_EDGE ( 'NONE', *, *, #15724, .T. ) ;
#3702 = VECTOR ( 'NONE', #2301, 1000.000000000000000 ) ;
#3703 = VERTEX_POINT ( 'NONE', #22421 ) ;
#3704 = CONTEXT_DEPENDENT_SHAPE_REPRESENTATION ( #12116, #19966 ) ;
#3705 = VERTEX_POINT ( 'NONE', #15171 ) ;
#3706 = CARTESIAN_POINT ( 'NONE',  ( 30.68762588338046982, -45.64284848299539732, -3.000000000000000000 ) ) ;
#3707 = EDGE_CURVE ( 'NONE', #11452, #13972, #6570, .T. ) ;
#3709 = EDGE_CURVE ( 'NONE', #9630, #14839, #12782, .T. ) ;
#3708 = CIRCLE ( 'NONE', #20441, 1.499999999999998668 ) ;
#3710 = AXIS2_PLACEMENT_3D ( 'NONE', #10334, #19864, #5207 ) ;
#3711 = CARTESIAN_POINT ( 'NONE',  ( -9.500000000000000000, -6.482511860946779655E-13, 10.20674201446023233 ) ) ;
#3712 = VERTEX_POINT ( 'NONE', #14942 ) ;
#3713 = CARTESIAN_POINT ( 'NONE',  ( 69.63636363636364024, 7.491529369508391930E-15, 0.000000000000000000 ) ) ;
#3714 = DIRECTION ( 'NONE',  ( -1.000000000000000000, 0.000000000000000000, 0.000000000000000000 ) ) ;
#3715 = ORIENTED_EDGE ( 'NONE', *, *, #9732, .T. ) ;
#3716 = DIRECTION ( 'NONE',  ( -1.000000000000000000, 0.000000000000000000, 0.000000000000000000 ) ) ;
#3717 = CARTESIAN_POINT ( 'NONE',  ( -6.153822176767817416E-13, 9.500000000000000000, -2.559589141758142894 ) ) ;
#3718 = AXIS2_PLACEMENT_3D ( 'NONE', #17221, #2231, #15392 ) ;
#3719 = CYLINDRICAL_SURFACE ( 'NONE', #16961, 49.99999999999998579 ) ;
#3720 = CIRCLE ( 'NONE', #19316, 5.000000000000007994 ) ;
#3721 = DIRECTION ( 'NONE',  ( 0.7071067811865457964, 8.659560562354910671E-17, -0.7071067811865492381 ) ) ;
#3722 = LINE ( 'NONE', #3952, #9862 ) ;
#3723 = CARTESIAN_POINT ( 'NONE',  ( -1.999999999999996669, 45.00000000000000000, -8.673617379884035472E-16 ) ) ;
#3724 = ADVANCED_FACE ( 'NONE', ( #4347 ), #18300, .T. ) ;
#3725 = CARTESIAN_POINT ( 'NONE',  ( -20.85000000000000853, 15.04000000000000092, -27.00000000000000000 ) ) ;
#3726 = VECTOR ( 'NONE', #21552, 1000.000000000000000 ) ;
#3727 = CIRCLE ( 'NONE', #13048, 5.999999999999998224 ) ;
#3728 = ORIENTED_EDGE ( 'NONE', *, *, #19908, .T. ) ;
#3729 = CARTESIAN_POINT ( 'NONE',  ( -5.622572944242076564E-13, 8.680847955711007202, 3.133165578109187166 ) ) ;
#3730 = ORIENTED_EDGE ( 'NONE', *, *, #5013, .T. ) ;
#3731 = ADVANCED_FACE ( 'NONE', ( #13730 ), #11755, .F. ) ;
#3732 = APPLICATION_PROTOCOL_DEFINITION ( 'draft international standard', 'automotive_design', 1998, #15693 ) ;
#3733 = VERTEX_POINT ( 'NONE', #23010 ) ;
#3734 = EDGE_LOOP ( 'NONE', ( #18235, #12409, #14416, #3544, #8809 ) ) ;
#3735 = EDGE_CURVE ( 'NONE', #1469, #21201, #769, .T. ) ;
#3736 = CARTESIAN_POINT ( 'NONE',  ( 0.000000000000000000, -14.96647757894464270, 7.750000000000000000 ) ) ;
#3737 = CARTESIAN_POINT ( 'NONE',  ( 5.365059087799946447, -7.384370330706356178, -12.33316557810918646 ) ) ;
#3738 = AXIS2_PLACEMENT_3D ( 'NONE', #10398, #12083, #1140 ) ;
#3739 = DIRECTION ( 'NONE',  ( 0.000000000000000000, 0.000000000000000000, -1.000000000000000000 ) ) ;
#3740 = VERTEX_POINT ( 'NONE', #19475 ) ;
#3741 = DIRECTION ( 'NONE',  ( 0.000000000000000000, 0.000000000000000000, 1.000000000000000000 ) ) ;
#3742 = LINE ( 'NONE', #20579, #10740 ) ;
#3743 = DIRECTION ( 'NONE',  ( 0.000000000000000000, 0.000000000000000000, 1.000000000000000000 ) ) ;
#3744 = FACE_OUTER_BOUND ( 'NONE', #18619, .T. ) ;
#3745 = CARTESIAN_POINT ( 'NONE',  ( 0.000000000000000000, -45.00000000000000000, 23.99999999999999645 ) ) ;
#3746 = EDGE_LOOP ( 'NONE', ( #12459, #17177, #4349 ) ) ;
#3747 = VECTOR ( 'NONE', #1625, 1000.000000000000000 ) ;
#3748 = DIRECTION ( 'NONE',  ( -1.000000000000000000, 0.000000000000000000, 0.000000000000000000 ) ) ;
#3749 = EDGE_LOOP ( 'NONE', ( #4895, #9749, #23837 ) ) ;
#3750 = VERTEX_POINT ( 'NONE', #6284 ) ;
#3751 = CARTESIAN_POINT ( 'NONE',  ( 68.18181818181818699, 7.491529369508391930E-15, 0.000000000000000000 ) ) ;
#3752 = CARTESIAN_POINT ( 'NONE',  ( -42.00000000000000000, 25.22443390181683043, -1.500000000000000000 ) ) ;
#3753 = CARTESIAN_POINT ( 'NONE',  ( 9.500000000000000000, 1.163414459189985485E-15, 3.499999999999999556 ) ) ;
#3754 = DIRECTION ( 'NONE',  ( -0.4828336235133042775, -0.8757121056631643752, 0.000000000000000000 ) ) ;
#3755 = CARTESIAN_POINT ( 'NONE',  ( -2.999999999999999112, 111.0000000000000000, 80.99999999999998579 ) ) ;
#3756 = LINE ( 'NONE', #2279, #21163 ) ;
#3757 = ADVANCED_FACE ( 'NONE', ( #23272 ), #8480, .T. ) ;
#3758 = AXIS2_PLACEMENT_3D ( 'NONE', #20454, #18507, #9323 ) ;
#3759 = AXIS2_PLACEMENT_3D ( 'NONE', #21198, #7868, #2400 ) ;
#3760 = ORIENTED_EDGE ( 'NONE', *, *, #10035, .T. ) ;
#3761 = AXIS2_PLACEMENT_3D ( 'NONE', #23164, #10193, #22796 ) ;
#3762 = VERTEX_POINT ( 'NONE', #19726 ) ;
#3763 = CARTESIAN_POINT ( 'NONE',  ( -6.822232771736903637E-13, 9.988891130263535700, 11.70674201446023410 ) ) ;
#3764 = EDGE_CURVE ( 'NONE', #3090, #16565, #4715, .T. ) ;
#3765 = VERTEX_POINT ( 'NONE', #695 ) ;
#3766 = ORIENTED_EDGE ( 'NONE', *, *, #12254, .F. ) ;
#3767 = AXIS2_PLACEMENT_3D ( 'NONE', #142, #18675, #14995 ) ;
#3768 = DIRECTION ( 'NONE',  ( -1.000000000000000000, -0.000000000000000000, -0.000000000000000000 ) ) ;
#3769 = ORIENTED_EDGE ( 'NONE', *, *, #963, .F. ) ;
#3770 = DIRECTION ( 'NONE',  ( -1.000000000000000000, 0.000000000000000000, 0.000000000000000000 ) ) ;
#3771 = CARTESIAN_POINT ( 'NONE',  ( 40.23082370883260239, 27.62204025492844650, -3.000000000000000000 ) ) ;
#3772 = SURFACE_STYLE_FILL_AREA ( #5365 ) ;
#3773 = DIRECTION ( 'NONE',  ( 0.000000000000000000, -1.000000000000000000, 0.000000000000000000 ) ) ;
#3774 = AXIS2_PLACEMENT_3D ( 'NONE', #19312, #4671, #1135 ) ;
#3775 = EDGE_LOOP ( 'NONE', ( #9540, #21194, #22865, #2504 ) ) ;
#3776 = DIRECTION ( 'NONE',  ( 1.000000000000000000, 0.000000000000000000, 0.000000000000000000 ) ) ;
#3777 = EDGE_LOOP ( 'NONE', ( #22753, #13218, #21350, #18119, #15431 ) ) ;
#3778 = FACE_OUTER_BOUND ( 'NONE', #3992, .T. ) ;
#3779 = LINE ( 'NONE', #12798, #23143 ) ;
#3780 = DIRECTION ( 'NONE',  ( -0.000000000000000000, -0.000000000000000000, -1.000000000000000000 ) ) ;
#3781 = CYLINDRICAL_SURFACE ( 'NONE', #11432, 8.000000000000000000 ) ;
#3782 =( BOUNDED_CURVE ( )  B_SPLINE_CURVE ( 2, ( #24024, #3410, #1226, #5363, #23784, #6836, #16438, #21724, #12667, #20247, #5016 ),
 .UNSPECIFIED., .F., .T. ) 
 B_SPLINE_CURVE_WITH_KNOTS ( ( 3, 2, 2, 2, 2, 3 ),
 ( 0.8000000000000000444, 0.8199999999999999512, 0.8399999999999999689, 0.8599999999999999867, 0.8800000000000000044, 0.9000000000000000222 ),
 .UNSPECIFIED. ) 
 CURVE ( )  GEOMETRIC_REPRESENTATION_ITEM ( )  RATIONAL_B_SPLINE_CURVE ( ( 1.000000000000000000, 0.9510565162951535312, 1.000000000000000000, 0.9510565162951535312, 1.000000000000000000, 0.9510565162951535312, 1.000000000000000000, 0.9510565162951535312, 1.000000000000000000, 0.9510565162951535312, 1.000000000000000000 ) ) 
 REPRESENTATION_ITEM ( '' )  );
#3783 = CARTESIAN_POINT ( 'NONE',  ( 83.30704456891035647, -5.000000000000000000, 6.123233995736775157E-16 ) ) ;
#3784 = CARTESIAN_POINT ( 'NONE',  ( 2.682529543900284974, -8.255977015246234174, -10.23316557810918859 ) ) ;
#3785 = DIRECTION ( 'NONE',  ( 0.000000000000000000, 0.000000000000000000, 1.000000000000000000 ) ) ;
#3786 = EDGE_CURVE ( 'NONE', #3740, #13716, #9935, .T. ) ;
#3787 = EDGE_LOOP ( 'NONE', ( #11016, #14336 ) ) ;
#3788 = DIRECTION ( 'NONE',  ( 0.000000000000000000, 0.000000000000000000, 1.000000000000000000 ) ) ;
#3789 = ORIENTED_EDGE ( 'NONE', *, *, #22915, .F. ) ;
#3790 = CARTESIAN_POINT ( 'NONE',  ( -41.49999999999999289, 27.79189783386526358, -27.00000000000000000 ) ) ;
#3791 = EDGE_CURVE ( 'NONE', #15261, #4197, #6546, .T. ) ;
#3792 = EDGE_CURVE ( 'NONE', #6922, #16055, #3006, .T. ) ;
#3793 = ORIENTED_EDGE ( 'NONE', *, *, #7425, .T. ) ;
#3794 = CARTESIAN_POINT ( 'NONE',  ( 0.000000000000000000, 0.000000000000000000, 0.000000000000000000 ) ) ;
#3795 = CARTESIAN_POINT ( 'NONE',  ( -23.90000000000000213, 29.49999999999999645, 0.000000000000000000 ) ) ;
#3796 = DIRECTION ( 'NONE',  ( -1.000000000000000000, -0.000000000000000000, -0.000000000000000000 ) ) ;
#3797 = LINE ( 'NONE', #10358, #7520 ) ;
#3798 = CARTESIAN_POINT ( 'NONE',  ( 5.871322893123449127, 8.081182679344781405, -6.359589141758142716 ) ) ;
#3799 = ORIENTED_EDGE ( 'NONE', *, *, #18905, .T. ) ;
#3800 = PLANE ( 'NONE',  #13430 ) ;
#3801 = CARTESIAN_POINT ( 'NONE',  ( 0.000000000000000000, 15.23000000000000220, 27.00000000000000000 ) ) ;
#3802 = VERTEX_POINT ( 'NONE', #21177 ) ;
#3803 = CARTESIAN_POINT ( 'NONE',  ( -6.822232771736904647E-13, 9.988891130263535700, 5.706742014460233214 ) ) ;
#3804 = ADVANCED_FACE ( 'NONE', ( #15808 ), #14385, .F. ) ;
#3805 = ORIENTED_EDGE ( 'NONE', *, *, #4003, .F. ) ;
#3806 = FACE_OUTER_BOUND ( 'NONE', #16811, .T. ) ;
#3807 = FACE_OUTER_BOUND ( 'NONE', #1575, .T. ) ;
#3808 = ADVANCED_FACE ( 'NONE', ( #12119 ), #16035, .T. ) ;
#3809 = CARTESIAN_POINT ( 'NONE',  ( 87.96568270381690979, -4.999999999999989342, 0.000000000000000000 ) ) ;
#3810 = VERTEX_POINT ( 'NONE', #15925 ) ;
#3811 = PLANE ( 'NONE',  #21056 ) ;
#3812 = PRODUCT_DEFINITION_SHAPE ( 'NONE', 'NONE',  #24124 ) ;
#3813 = CARTESIAN_POINT ( 'NONE',  ( 41.50000000000000000, -28.80990663662250739, 11.00000000000000000 ) ) ;
#3814 = EDGE_CURVE ( 'NONE', #5416, #569, #5825, .T. ) ;
#3815 = ADVANCED_FACE ( 'NONE', ( #23386 ), #23140, .T. ) ;
#3816 = ADVANCED_FACE ( 'NONE', ( #13866 ), #13609, .T. ) ;
#3817 = CARTESIAN_POINT ( 'NONE',  ( 23.00000000000000000, 12.00453763395397466, 7.608955687739546114 ) ) ;
#3818 = LINE ( 'NONE', #11473, #4399 ) ;
#3819 = EDGE_LOOP ( 'NONE', ( #1203, #1901, #14356, #15271 ) ) ;
#3820 = AXIS2_PLACEMENT_3D ( 'NONE', #16199, #16416, #14822 ) ;
#3821 = AXIS2_PLACEMENT_3D ( 'NONE', #10512, #2725, #5050 ) ;
#3822 = CONTEXT_DEPENDENT_SHAPE_REPRESENTATION ( #2166, #16770 ) ;
#3823 = EDGE_LOOP ( 'NONE', ( #1028, #20674, #15851, #5881 ) ) ;
#3824 = DIRECTION ( 'NONE',  ( 0.000000000000000000, 0.000000000000000000, -1.000000000000000000 ) ) ;
#3825 = CARTESIAN_POINT ( 'NONE',  ( -2.935661446562617183, 9.035036904803758873, 9.806742014460233747 ) ) ;
#3826 = VERTEX_POINT ( 'NONE', #21545 ) ;
#3827 = FACE_OUTER_BOUND ( 'NONE', #21662, .T. ) ;
#3828 = CIRCLE ( 'NONE', #21766, 4.249999999999996447 ) ;
#3829 = ORIENTED_EDGE ( 'NONE', *, *, #21127, .T. ) ;
#3830 = DIRECTION ( 'NONE',  ( -0.000000000000000000, -0.000000000000000000, -1.000000000000000000 ) ) ;
#3831 = ADVANCED_FACE ( 'NONE', ( #21311 ), #8343, .F. ) ;
#3832 = CARTESIAN_POINT ( 'NONE',  ( 0.000000000000000000, 0.000000000000000000, 15.50000000000000000 ) ) ;
#3833 = CARTESIAN_POINT ( 'NONE',  ( 84.76159002345582394, -1.078520768856852078E-29, 5.000000000000007994 ) ) ;
#3834 = DIRECTION ( 'NONE',  ( -1.000000000000000000, -0.000000000000000000, -0.000000000000000000 ) ) ;
#3835 = CIRCLE ( 'NONE', #20981, 1.000000000000000000 ) ;
#3836 = CARTESIAN_POINT ( 'NONE',  ( 1.999999999999994449, 45.00000000000000000, 23.99999999999999645 ) ) ;
#3837 = ORIENTED_EDGE ( 'NONE', *, *, #5281, .T. ) ;
#3838 = EDGE_LOOP ( 'NONE', ( #19352, #5352, #15020, #1342 ) ) ;
#3839 = DIRECTION ( 'NONE',  ( 1.000000000000000000, 0.000000000000000000, 0.000000000000000000 ) ) ;
#3840 = DIRECTION ( 'NONE',  ( 0.000000000000000000, 0.000000000000000000, 1.000000000000000000 ) ) ;
#3841 = CARTESIAN_POINT ( 'NONE',  ( 5.871322893124553133, -8.081182679343980269, -8.906742014460233392 ) ) ;
#3842 = LINE ( 'NONE', #1650, #22845 ) ;
#3843 = EDGE_CURVE ( 'NONE', #1819, #578, #12844, .T. ) ;
#3844 = VERTEX_POINT ( 'NONE', #14203 ) ;
#3845 = CARTESIAN_POINT ( 'NONE',  ( -8.680847955711200825, 2.820578480813073607, 3.533165578109187965 ) ) ;
#3846 = ORIENTED_EDGE ( 'NONE', *, *, #10438, .F. ) ;
#3847 = CLOSED_SHELL ( 'NONE', ( #21423, #3174, #14767, #13187, #8286, #4679, #21159, #17566, #12323, #17976, #7985, #13752, #10821, #1816, #7327, #18525, #23038, #10281, #1535, #8413, #3804, #10791, #7223, #9782, #23463, #19552, #6576, #17550, #21702, #14865, #7168, #11415, #17068, #9235, #8943, #6069, #5441, #4126, #6178, #10336, #14481, #22171, #23191, #1659, #5327, #5725, #3149, #16986, #17232, #18784, #4191, #17763, #8442, #10782, #10359, #13638, #6441, #3235, #18818, #21830, #20365, #10471, #14537, #14980, #1229, #11476, #8648, #2544, #16056, #7053, #5948, #10010, #9327, #6955, #19076, #14662, #4189, #4201, #217, #3731, #14080, #22731, #8646, #18471, #11086, #12825, #14591, #14304, #6334, #7226, #705, #9992, #3102, #12888, #6959, #17749, #13786, #16402, #5597, #13612, #14574, #15390, #1934, #20135, #21094, #2426, #6713, #11844, #4331, #9818, #23923, #3401, #19809, #961, #6496, #4281, #9176, #3481, #22547, #17213, #12583, #14317, #9248, #20517, #18565, #8743, #15583 ) ) ;
#3848 = SHAPE_DEFINITION_REPRESENTATION ( #2806, #2057 ) ;
#3849 = ORIENTED_EDGE ( 'NONE', *, *, #6533, .F. ) ;
#3850 = VERTEX_POINT ( 'NONE', #12737 ) ;
#3851 = CARTESIAN_POINT ( 'NONE',  ( 58.57977184163763695, 7.562528597612068045E-15, 0.000000000000000000 ) ) ;
#3852 = CARTESIAN_POINT ( 'NONE',  ( -8.680847955710813579, -2.820578480814258437, -7.733165578109187699 ) ) ;
#3853 = DIRECTION ( 'NONE',  ( 0.000000000000000000, -9.256405414277000802E-16, -1.000000000000000000 ) ) ;
#3854 = ORIENTED_EDGE ( 'NONE', *, *, #9226, .T. ) ;
#3855 = CARTESIAN_POINT ( 'NONE',  ( -31.74999999999995737, 0.000000000000000000, 0.000000000000000000 ) ) ;
#3856 = DIRECTION ( 'NONE',  ( -0.8757121056631641531, 0.4828336235133042775, 0.000000000000000000 ) ) ;
#3857 = CARTESIAN_POINT ( 'NONE',  ( 58.57977184163763695, 5.000000000000015099, 0.000000000000000000 ) ) ;
#3858 = CARTESIAN_POINT ( 'NONE',  ( -40.66734255040739043, 26.56420859267092283, -1.500000000000000000 ) ) ;
#3859 = CARTESIAN_POINT ( 'NONE',  ( 3.890962118697714531E-15, 15.50000000000000000, 19.20000000000000995 ) ) ;
#3860 = FACE_OUTER_BOUND ( 'NONE', #2113, .T. ) ;
#3861 = EDGE_LOOP ( 'NONE', ( #11961, #6796, #7209, #13340 ) ) ;
#3862 = EDGE_CURVE ( 'NONE', #18287, #10867, #18869, .T. ) ;
#3863 = EDGE_LOOP ( 'NONE', ( #13655, #6070, #18703, #1852 ) ) ;
#3864 = CARTESIAN_POINT ( 'NONE',  ( 60.90909090909091361, 7.491529369508391930E-15, 0.000000000000000000 ) ) ;
#3865 = CARTESIAN_POINT ( 'NONE',  ( -42.62132034355964549, 25.48082444701821103, -1.614108343103369153E-16 ) ) ;
#3866 = DIRECTION ( 'NONE',  ( 0.000000000000000000, 0.000000000000000000, 1.000000000000000000 ) ) ;
#3867 = CARTESIAN_POINT ( 'NONE',  ( -42.00000000000000000, -4.000000000000000888, 8.500000000000000000 ) ) ;
#3868 = FACE_OUTER_BOUND ( 'NONE', #15410, .T. ) ;
#3869 = DIRECTION ( 'NONE',  ( 0.7071067811865500152, 0.000000000000000000, -0.7071067811865450192 ) ) ;
#3870 = ADVANCED_FACE ( 'NONE', ( #1423 ), #17705, .T. ) ;
#3871 = CARTESIAN_POINT ( 'NONE',  ( 5.871322893124551356, -8.081182679343980269, 8.906742014460233392 ) ) ;
#3872 = ORIENTED_EDGE ( 'NONE', *, *, #15324, .T. ) ;
#3873 = ORIENTED_EDGE ( 'NONE', *, *, #241, .F. ) ;
#3874 = APPLICATION_CONTEXT ( 'automotive_design' ) ;
#3875 = AXIS2_PLACEMENT_3D ( 'NONE', #19230, #6422, #17885 ) ;
#3876 = EDGE_LOOP ( 'NONE', ( #18717, #19465, #21892, #19014, #11409 ) ) ;
#3877 = ORIENTED_EDGE ( 'NONE', *, *, #5504, .T. ) ;
#3878 = ORIENTED_EDGE ( 'NONE', *, *, #17361, .T. ) ;
#3879 = CARTESIAN_POINT ( 'NONE',  ( 59.45454545454545325, 7.491529369508391930E-15, 0.000000000000000000 ) ) ;
#3880 = CARTESIAN_POINT ( 'NONE',  ( 6.809999908187194197E-13, -9.988891130263535700, 9.559589141758145558 ) ) ;
#3881 = AXIS2_PLACEMENT_3D ( 'NONE', #19953, #12263, #8720 ) ;
#3882 = LINE ( 'NONE', #237, #9864 ) ;
#3883 = DIRECTION ( 'NONE',  ( 1.000000000000000000, 0.000000000000000000, 0.000000000000000000 ) ) ;
#3884 = DIRECTION ( 'NONE',  ( 1.000000000000000000, 0.000000000000000000, 0.000000000000000000 ) ) ;
#3885 = DIRECTION ( 'NONE',  ( -1.000000000000000000, -0.000000000000000000, -0.000000000000000000 ) ) ;
#3886 = EDGE_CURVE ( 'NONE', #5851, #14876, #3469, .T. ) ;
#3887 = VERTEX_POINT ( 'NONE', #11000 ) ;
#3888 = EDGE_CURVE ( 'NONE', #3699, #10247, #14694, .T. ) ;
#3889 = DIRECTION ( 'NONE',  ( -1.000000000000000000, 0.000000000000000000, 0.000000000000000000 ) ) ;
#3890 = CYLINDRICAL_SURFACE ( 'NONE', #19965, 5.000000000000000888 ) ;
#3891 = CARTESIAN_POINT ( 'NONE',  ( -17.06033556854818656, 8.068938288216804366, 5.036196554528638458 ) ) ;
#3892 = EDGE_CURVE ( 'NONE', #7789, #19210, #16906, .T. ) ;
#3893 = CARTESIAN_POINT ( 'NONE',  ( 42.00000000000000000, 26.82133436441678853, 12.00000000000000000 ) ) ;
#3894 = VERTEX_POINT ( 'NONE', #8715 ) ;
#3895 = CARTESIAN_POINT ( 'NONE',  ( 8.680847955711199049, -2.820578480813074496, -6.533165578109188409 ) ) ;
#3896 = DIRECTION ( 'NONE',  ( -0.000000000000000000, -0.000000000000000000, -1.000000000000000000 ) ) ;
#3897 = ORIENTED_EDGE ( 'NONE', *, *, #8866, .F. ) ;
#3898 = CYLINDRICAL_SURFACE ( 'NONE', #11849, 9.500000000000000000 ) ;
#3899 = ORIENTED_EDGE ( 'NONE', *, *, #4858, .F. ) ;
#3900 = AXIS2_PLACEMENT_3D ( 'NONE', #4915, #12329, #19797 ) ;
#3901 = DIRECTION ( 'NONE',  ( -1.000000000000000000, -0.000000000000000000, -0.000000000000000000 ) ) ;
#3902 = VERTEX_POINT ( 'NONE', #7006 ) ;
#3903 = CARTESIAN_POINT ( 'NONE',  ( 0.000000000000000000, 15.03999999999999737, 2.200000000000000178 ) ) ;
#3904 = DIRECTION ( 'NONE',  ( 0.000000000000000000, -1.224646799147353207E-16, 1.000000000000000000 ) ) ;
#3905 = DIRECTION ( 'NONE',  ( 0.000000000000000000, 0.000000000000000000, 1.000000000000000000 ) ) ;
#3906 = LINE ( 'NONE', #2201, #16568 ) ;
#3907 = CARTESIAN_POINT ( 'NONE',  ( 0.000000000000000000, 0.000000000000000000, 12.00000000000000000 ) ) ;
#3908 = DIRECTION ( 'NONE',  ( 1.000000000000000000, 0.000000000000000000, 0.000000000000000000 ) ) ;
#3909 = CARTESIAN_POINT ( 'NONE',  ( 7.685661446561619314, 5.583959896779020049, -10.25958914175814485 ) ) ;
#3910 = EDGE_LOOP ( 'NONE', ( #23048, #18492 ) ) ;
#3911 = VECTOR ( 'NONE', #21380, 1000.000000000000000 ) ;
#3912 = DIRECTION ( 'NONE',  ( 1.000000000000000000, 0.000000000000000000, 0.000000000000000000 ) ) ;
#3913 = ADVANCED_FACE ( 'NONE', ( #18477 ), #10671, .T. ) ;
#3914 = EDGE_CURVE ( 'NONE', #21873, #10579, #13802, .T. ) ;
#3915 = ORIENTED_EDGE ( 'NONE', *, *, #21862, .T. ) ;
#3916 = CARTESIAN_POINT ( 'NONE',  ( 9.499999999999790390, 3.086737114213260025, 5.306742014460231971 ) ) ;
#3917 = CARTESIAN_POINT ( 'NONE',  ( -7.561939491010504000, 5.750397476200735269, 11.99999999999999822 ) ) ;
#3918 = LINE ( 'NONE', #4293, #8898 ) ;
#3919 = DIRECTION ( 'NONE',  ( -0.000000000000000000, -0.000000000000000000, -1.000000000000000000 ) ) ;
#3920 = DIRECTION ( 'NONE',  ( -1.000000000000000000, 0.000000000000000000, -0.000000000000000000 ) ) ;
#3921 = FACE_OUTER_BOUND ( 'NONE', #2652, .T. ) ;
#3922 = DIRECTION ( 'NONE',  ( 1.000000000000000000, 0.000000000000000000, 0.000000000000000000 ) ) ;
#3923 = ORIENTED_EDGE ( 'NONE', *, *, #6310, .T. ) ;
#3924 = FACE_OUTER_BOUND ( 'NONE', #10986, .T. ) ;
#3925 = LINE ( 'NONE', #11108, #23863 ) ;
#3926 = CARTESIAN_POINT ( 'NONE',  ( 2.454813078130514813E-15, -16.67999999999999972, 13.50000000000000178 ) ) ;
#3927 = DIRECTION ( 'NONE',  ( -0.000000000000000000, -0.000000000000000000, -1.000000000000000000 ) ) ;
#3928 = CIRCLE ( 'NONE', #11691, 18.50000000000000000 ) ;
#3929 = ORIENTED_EDGE ( 'NONE', *, *, #9606, .F. ) ;
#3930 = ORIENTED_EDGE ( 'NONE', *, *, #2375, .F. ) ;
#3931 = ADVANCED_FACE ( 'NONE', ( #1765 ), #18350, .T. ) ;
#3932 = ITEM_DEFINED_TRANSFORMATION ( 'NONE', 'NONE', #20142,  #8005 ) ;
#3933 = ORIENTED_EDGE ( 'NONE', *, *, #3380, .T. ) ;
#3934 = DIRECTION ( 'NONE',  ( 0.9160001545545232160, 0.4011779117250717785, 0.000000000000000000 ) ) ;
#3935 = CARTESIAN_POINT ( 'NONE',  ( -2.024999999999999911, 45.00000000000000000, 27.00000000000000000 ) ) ;
#3936 = EDGE_CURVE ( 'NONE', #14543, #5778, #7249, .T. ) ;
#3937 = LINE ( 'NONE', #5887, #4024 ) ;
#3938 = ORIENTED_EDGE ( 'NONE', *, *, #18494, .F. ) ;
#3939 = ORIENTED_EDGE ( 'NONE', *, *, #23322, .T. ) ;
#3940 = EDGE_CURVE ( 'NONE', #14296, #2924, #6409, .T. ) ;
#3941 = EDGE_CURVE ( 'NONE', #20601, #5111, #2109, .T. ) ;
#3942 = DIRECTION ( 'NONE',  ( 0.5735764363510424957, 0.8191520442889943521, 0.000000000000000000 ) ) ;
#3943 = ORIENTED_EDGE ( 'NONE', *, *, #19409, .T. ) ;
#3944 = VECTOR ( 'NONE', #15602, 1000.000000000000000 ) ;
#3945 = ORIENTED_EDGE ( 'NONE', *, *, #22475, .T. ) ;
#3946 = CARTESIAN_POINT ( 'NONE',  ( -9.499999999999799272, -3.086737114213243593, 10.30674201446023019 ) ) ;
#3947 = FACE_OUTER_BOUND ( 'NONE', #23258, .T. ) ;
#3948 = AXIS2_PLACEMENT_3D ( 'NONE', #15674, #13989, #3238 ) ;
#3949 = CYLINDRICAL_SURFACE ( 'NONE', #23146, 5.000000000000000888 ) ;
#3950 = DIRECTION ( 'NONE',  ( 0.000000000000000000, 0.000000000000000000, -1.000000000000000000 ) ) ;
#3951 = EDGE_LOOP ( 'NONE', ( #7215, #10549, #3281, #7774 ) ) ;
#3952 = CARTESIAN_POINT ( 'NONE',  ( -40.66734255040739043, 26.56420859267092283, -3.000000000000000000 ) ) ;
#3953 = LINE ( 'NONE', #12099, #22358 ) ;
#3954 = CARTESIAN_POINT ( 'NONE',  ( 31.49999999999999289, -51.00000000000000711, 12.50000000000000000 ) ) ;
#3955 = ORIENTED_EDGE ( 'NONE', *, *, #11637, .F. ) ;
#3956 = VERTEX_POINT ( 'NONE', #14431 ) ;
#3957 = CARTESIAN_POINT ( 'NONE',  ( 7.022953521755574080, -5.102474405759714671, 4.433165578109187877 ) ) ;
#3958 = EDGE_LOOP ( 'NONE', ( #19542, #1797, #15613, #17708 ) ) ;
#3959 = APPLICATION_PROTOCOL_DEFINITION ( 'draft international standard', 'automotive_design', 1998, #14630 ) ;
#3960 = EDGE_CURVE ( 'NONE', #20194, #8068, #22111, .T. ) ;
#3961 = AXIS2_PLACEMENT_3D ( 'NONE', #7767, #9841, #2182 ) ;
#3962 = VERTEX_POINT ( 'NONE', #6903 ) ;
#3963 = ORIENTED_EDGE ( 'NONE', *, *, #15057, .T. ) ;
#3964 = DIRECTION ( 'NONE',  ( 0.000000000000000000, -0.000000000000000000, -1.000000000000000000 ) ) ;
#3965 = CARTESIAN_POINT ( 'NONE',  ( -5.365059087799947335, 7.384370330706355290, -7.333165578109188232 ) ) ;
#3966 = CIRCLE ( 'NONE', #1626, 17.87500000001787726 ) ;
#3967 = LINE ( 'NONE', #17019, #6384 ) ;
#3968 = ORIENTED_EDGE ( 'NONE', *, *, #8845, .F. ) ;
#3969 = CYLINDRICAL_SURFACE ( 'NONE', #14194, 1.500000000000001332 ) ;
#3970 = CARTESIAN_POINT ( 'NONE',  ( 9.500000000000000000, 1.163414459189985485E-15, 12.50000000000000000 ) ) ;
#3971 = EDGE_CURVE ( 'NONE', #2260, #10767, #20931, .T. ) ;
#3972 = DIRECTION ( 'NONE',  ( 1.000000000000000000, 0.000000000000000000, 0.000000000000000000 ) ) ;
#3973 = EDGE_CURVE ( 'NONE', #8446, #6823, #6115, .T. ) ;
#3974 = CARTESIAN_POINT ( 'NONE',  ( 89.12522638709219791, -5.000000000000000888, 6.123233995736776143E-16 ) ) ;
#3975 = B_SPLINE_CURVE_WITH_KNOTS ( 'NONE', 3,
 ( #2585, #23335, #16581, #12909 ),
 .UNSPECIFIED., .F., .F.,
 ( 4, 4 ),
 ( 0.000000000000000000, 0.001795700496623673509 ),
 .UNSPECIFIED. ) ;
#3976 = FACE_OUTER_BOUND ( 'NONE', #6159, .T. ) ;
#3977 = CARTESIAN_POINT ( 'NONE',  ( 0.000000000000000000, 15.23000000000000220, 27.00000000000000000 ) ) ;
#3978 = CARTESIAN_POINT ( 'NONE',  ( 9.500000000000000000, 1.163414459189985485E-15, 12.50000000000000000 ) ) ;
#3979 = CARTESIAN_POINT ( 'NONE',  ( 28.99999999999998579, -29.49999999999999645, 0.000000000000000000 ) ) ;
#3980 = AXIS2_PLACEMENT_3D ( 'NONE', #16419, #7161, #19869 ) ;
#3981 = AXIS2_PLACEMENT_3D ( 'NONE', #3015, #7013, #15932 ) ;
#3982 = DIRECTION ( 'NONE',  ( 0.000000000000000000, -1.000000000000000000, 0.000000000000000000 ) ) ;
#3983 = CARTESIAN_POINT ( 'NONE',  ( 9.000000000000000000, 1.102182119232617714E-15, 103.9999999999999858 ) ) ;
#3984 = AXIS2_PLACEMENT_3D ( 'NONE', #2467, #291, #17348 ) ;
#3985 = AXIS2_PLACEMENT_3D ( 'NONE', #15340, #4522, #17171 ) ;
#3986 = AXIS2_PLACEMENT_3D ( 'NONE', #16012, #21282, #1152 ) ;
#3987 = VECTOR ( 'NONE', #6394, 1000.000000000000000 ) ;
#3988 =( NAMED_UNIT ( * ) SI_UNIT ( $, .STERADIAN. ) SOLID_ANGLE_UNIT ( ) );
#3989 = ORIENTED_EDGE ( 'NONE', *, *, #18579, .F. ) ;
#3990 = ORIENTED_EDGE ( 'NONE', *, *, #22025, .F. ) ;
#3991 = CIRCLE ( 'NONE', #6737, 5.000000000000007994 ) ;
#3992 = EDGE_LOOP ( 'NONE', ( #20327, #20719, #11977 ) ) ;
#3993 = VERTEX_POINT ( 'NONE', #18131 ) ;
#3994 = CYLINDRICAL_SURFACE ( 'NONE', #14222, 1.999999999999994449 ) ;
#3995 = CARTESIAN_POINT ( 'NONE',  ( 0.000000000000000000, 15.03999999999999737, 2.200000000000000178 ) ) ;
#3996 = UNCERTAINTY_MEASURE_WITH_UNIT (LENGTH_MEASURE( 1.000000000000000082E-05 ), #19282, 'distance_accuracy_value', 'NONE');
#3997 = CARTESIAN_POINT ( 'NONE',  ( 9.500000000000000000, 6.470877716354879437E-13, -11.20674201446023410 ) ) ;
#3999 = VECTOR ( 'NONE', #18027, 1000.000000000000000 ) ;
#3998 = CARTESIAN_POINT ( 'NONE',  ( -31.74999999999995737, 0.000000000000000000, 5.000000000000000888 ) ) ;
#4000 = CARTESIAN_POINT ( 'NONE',  ( 7.685661446561619314, 5.583959896779020049, -5.406742014460233392 ) ) ;
#4001 = AXIS2_PLACEMENT_3D ( 'NONE', #16813, #20988, #13414 ) ;
#4002 = AXIS2_PLACEMENT_3D ( 'NONE', #17453, #14154, #21488 ) ;
#4003 = EDGE_CURVE ( 'NONE', #13451, #4173, #14322, .T. ) ;
#4004 = CIRCLE ( 'NONE', #9426, 20.85000000000000142 ) ;
#4005 = VECTOR ( 'NONE', #14888, 1000.000000000000000 ) ;
#4006 = FACE_OUTER_BOUND ( 'NONE', #22135, .T. ) ;
#4007 = ORIENTED_EDGE ( 'NONE', *, *, #9250, .T. ) ;
#4008 = AXIS2_PLACEMENT_3D ( 'NONE', #6907, #18244, #18135 ) ;
#4009 = CARTESIAN_POINT ( 'NONE',  ( 11.50000000000000000, -7.033831428820063181, -16.43291941292179104 ) ) ;
#4010 = CARTESIAN_POINT ( 'NONE',  ( 23.00000000000000000, 0.000000000000000000, 0.000000000000000000 ) ) ;
#4011 = CARTESIAN_POINT ( 'NONE',  ( 29.00000000000000000, 29.50000000000000000, 14.00000000000000178 ) ) ;
#4012 = AXIS2_PLACEMENT_3D ( 'NONE', #5914, #15536, #4101 ) ;
#4013 = LINE ( 'NONE', #474, #5174 ) ;
#4014 = APPLICATION_CONTEXT ( 'automotive_design' ) ;
#4015 = CARTESIAN_POINT ( 'NONE',  ( 6.809999908187194197E-13, -9.988891130263535700, 4.706742014460233214 ) ) ;
#4016 = EDGE_LOOP ( 'NONE', ( #12419, #5534, #5554, #11475 ) ) ;
#4017 = VERTEX_POINT ( 'NONE', #14562 ) ;
#4018 = CARTESIAN_POINT ( 'NONE',  ( 23.00000000000000000, -3.205857990849823480, 11.23818298448541420 ) ) ;
#4019 = ORIENTED_EDGE ( 'NONE', *, *, #18486, .F. ) ;
#4020 = AXIS2_PLACEMENT_3D ( 'NONE', #7743, #20692, #2149 ) ;
#4021 = CARTESIAN_POINT ( 'NONE',  ( 9.499999999999790390, 3.086737114213260025, 8.159589141758143427 ) ) ;
#4022 = CIRCLE ( 'NONE', #2471, 5.000000000000007994 ) ;
#4023 = ADVANCED_FACE ( 'NONE', ( #5312 ), #18710, .T. ) ;
#4024 = VECTOR ( 'NONE', #14688, 1000.000000000000000 ) ;
#4025 = ORIENTED_EDGE ( 'NONE', *, *, #2688, .F. ) ;
#4026 = CARTESIAN_POINT ( 'NONE',  ( 0.000000000000000000, 0.000000000000000000, 0.000000000000000000 ) ) ;
#4027 = AXIS2_PLACEMENT_3D ( 'NONE', #12417, #20700, #20838 ) ;
#4028 = DIRECTION ( 'NONE',  ( 0.5735764363510424957, 0.8191520442889943521, 0.000000000000000000 ) ) ;
#4029 = TOROIDAL_SURFACE ( 'NONE', #2865, 10.49999999999999822, 1.000000000000000000 ) ;
#4030 = FACE_OUTER_BOUND ( 'NONE', #2514, .T. ) ;
#4031 = EDGE_CURVE ( 'NONE', #19513, #11779, #7815, .T. ) ;
#4032 = CARTESIAN_POINT ( 'NONE',  ( 10.49999999999999822, 0.000000000000000000, 2.499999999999999556 ) ) ;
#4033 = CONICAL_SURFACE ( 'NONE', #20788, 5.000000000000007994, 0.9599310885968855844 ) ;
#4034 = DIRECTION ( 'NONE',  ( -0.000000000000000000, 0.000000000000000000, 1.000000000000000000 ) ) ;
#4035 = EDGE_CURVE ( 'NONE', #19904, #21161, #1838, .T. ) ;
#4036 = FACE_OUTER_BOUND ( 'NONE', #18575, .T. ) ;
#4037 = LINE ( 'NONE', #13552, #22689 ) ;
#4038 = ORIENTED_EDGE ( 'NONE', *, *, #16243, .T. ) ;
#4039 = FACE_OUTER_BOUND ( 'NONE', #14974, .T. ) ;
#4040 = EDGE_LOOP ( 'NONE', ( #10842, #1633, #18628, #7371 ) ) ;
#4041 = DIRECTION ( 'NONE',  ( 1.000000000000000000, 0.000000000000000000, 0.000000000000000000 ) ) ;
#4042 = CIRCLE ( 'NONE', #10266, 8.000000000000003553 ) ;
#4043 = CARTESIAN_POINT ( 'NONE',  ( 2.903090122117997218, 8.519021868010421272, 80.21852650458262701 ) ) ;
#4044 = CARTESIAN_POINT ( 'NONE',  ( 23.00000000000000000, 5.985147671565880678, -12.89120389306408754 ) ) ;
#4045 = CIRCLE ( 'NONE', #19239, 4.499999999999997335 ) ;
#4046 = AXIS2_PLACEMENT_3D ( 'NONE', #3000, #6541, #23382 ) ;
#4047 = CARTESIAN_POINT ( 'NONE',  ( -29.00000000000000000, -29.49999999999999645, 11.50000000000000000 ) ) ;
#4048 = CIRCLE ( 'NONE', #13393, 18.50000000000000000 ) ;
#4049 = CARTESIAN_POINT ( 'NONE',  ( -2.382914664853783560, 8.679543164111374054, 79.16706182717918239 ) ) ;
#4050 = CIRCLE ( 'NONE', #20808, 8.000000000000000000 ) ;
#4051 = DIRECTION ( 'NONE',  ( 1.000000000000000000, 1.224606353822377258E-16, 0.000000000000000000 ) ) ;
#4052 = FACE_OUTER_BOUND ( 'NONE', #3188, .T. ) ;
#4053 = DIRECTION ( 'NONE',  ( -0.000000000000000000, -0.000000000000000000, 1.000000000000000000 ) ) ;
#4054 = CIRCLE ( 'NONE', #13011, 0.9599481167642566204 ) ;
#4055 = ORIENTED_EDGE ( 'NONE', *, *, #13933, .F. ) ;
#4056 = PLANE ( 'NONE',  #14803 ) ;
#4057 = DIRECTION ( 'NONE',  ( -1.000000000000000000, 0.000000000000000000, 0.000000000000000000 ) ) ;
#4058 = EDGE_CURVE ( 'NONE', #6887, #9582, #2212, .T. ) ;
#4059 = DIRECTION ( 'NONE',  ( -0.000000000000000000, -0.000000000000000000, -1.000000000000000000 ) ) ;
#4060 = ORIENTED_EDGE ( 'NONE', *, *, #21675, .T. ) ;
#4061 = EDGE_CURVE ( 'NONE', #14, #10814, #22934, .T. ) ;
#4062 = EDGE_CURVE ( 'NONE', #4924, #5717, #11609, .T. ) ;
#4063 = ORIENTED_EDGE ( 'NONE', *, *, #15668, .T. ) ;
#4064 = CIRCLE ( 'NONE', #17701, 5.000000000000007994 ) ;
#4065 = AXIS2_PLACEMENT_3D ( 'NONE', #16812, #22468, #5748 ) ;
#4066 = CONTEXT_DEPENDENT_SHAPE_REPRESENTATION ( #4343, #16260 ) ;
#4068 = ORIENTED_EDGE ( 'NONE', *, *, #5566, .F. ) ;
#4067 = CIRCLE ( 'NONE', #11038, 5.000000000000007994 ) ;
#4069 = DIRECTION ( 'NONE',  ( -1.000000000000000000, 0.000000000000000000, 0.000000000000000000 ) ) ;
#4070 = AXIS2_PLACEMENT_3D ( 'NONE', #2640, #10051, #4602 ) ;
#4071 = CIRCLE ( 'NONE', #16137, 0.9999999999999994449 ) ;
#4072 = DIRECTION ( 'NONE',  ( 0.7071067811865474617, 0.000000000000000000, 0.7071067811865474617 ) ) ;
#4073 = ORIENTED_EDGE ( 'NONE', *, *, #2401, .F. ) ;
#4074 = CIRCLE ( 'NONE', #200, 8.000000000000000000 ) ;
#4075 = ORIENTED_EDGE ( 'NONE', *, *, #21500, .T. ) ;
#4076 = FACE_OUTER_BOUND ( 'NONE', #3550, .T. ) ;
#4077 = VERTEX_POINT ( 'NONE', #5784 ) ;
#4078 = CARTESIAN_POINT ( 'NONE',  ( -6.575584573473629568, -6.878740310043753858, -3.499821620521013976 ) ) ;
#4079 = EDGE_LOOP ( 'NONE', ( #13477, #3520, #1781, #293 ) ) ;
#4080 = DIRECTION ( 'NONE',  ( -1.000000000000000000, 0.000000000000000000, 0.000000000000000000 ) ) ;
#4081 = CARTESIAN_POINT ( 'NONE',  ( 29.00000000000000711, -29.50000000000000711, 27.00000000000000000 ) ) ;
#4082 = LINE ( 'NONE', #1991, #20024 ) ;
#4083 = VECTOR ( 'NONE', #4818, 1000.000000000000000 ) ;
#4084 = VECTOR ( 'NONE', #9617, 1000.000000000000000 ) ;
#4085 = DIRECTION ( 'NONE',  ( 1.000000000000000000, 1.224606353822377258E-16, 0.000000000000000000 ) ) ;
#4086 = EDGE_LOOP ( 'NONE', ( #17233, #2987, #16759, #1176 ) ) ;
#4087 = DIRECTION ( 'NONE',  ( 0.000000000000000000, -0.5406408174555868973, -0.8412535328311879779 ) ) ;
#4088 = LINE ( 'NONE', #5543, #2864 ) ;
#4089 = ORIENTED_EDGE ( 'NONE', *, *, #12668, .F. ) ;
#4090 = CIRCLE ( 'NONE', #9919, 9.000000000000000000 ) ;
#4091 = CARTESIAN_POINT ( 'NONE',  ( 8.680847955711199049, -2.820578480813074496, 4.533165578109188409 ) ) ;
#4092 = VERTEX_POINT ( 'NONE', #54 ) ;
#4093 = AXIS2_PLACEMENT_3D ( 'NONE', #22674, #20861, #8018 ) ;
#4094 = EDGE_CURVE ( 'NONE', #21063, #19544, #22256, .T. ) ;
#4095 = VERTEX_POINT ( 'NONE', #19077 ) ;
#4096 = ADVANCED_FACE ( 'NONE', ( #5890 ), #8094, .F. ) ;
#4097 = CYLINDRICAL_SURFACE ( 'NONE', #2930, 5.000000000000000888 ) ;
#4098 = AXIS2_PLACEMENT_3D ( 'NONE', #21575, #3031, #8610 ) ;
#4099 = ORIENTED_EDGE ( 'NONE', *, *, #22476, .F. ) ;
#4100 = ORIENTED_EDGE ( 'NONE', *, *, #15980, .T. ) ;
#4101 = DIRECTION ( 'NONE',  ( 1.000000000000000000, 0.000000000000000000, 0.000000000000000000 ) ) ;
#4102 = CARTESIAN_POINT ( 'NONE',  ( 7.022953521755574080, -5.102474405759714671, -10.43316557810918788 ) ) ;
#4103 = DIRECTION ( 'NONE',  ( -1.000000000000000000, -1.224606353822377258E-16, -0.000000000000000000 ) ) ;
#4104 = ORIENTED_EDGE ( 'NONE', *, *, #9021, .F. ) ;
#4105 = CARTESIAN_POINT ( 'NONE',  ( -9.000000000000000000, 1.102182119232617714E-15, 15.00000000000000178 ) ) ;
#4106 = FACE_OUTER_BOUND ( 'NONE', #3132, .T. ) ;
#4107 = DIRECTION ( 'NONE',  ( 1.000000000000000000, 1.224606353822377258E-16, 0.000000000000000000 ) ) ;
#4108 = DIRECTION ( 'NONE',  ( -1.000000000000000000, 0.000000000000000000, 0.000000000000000000 ) ) ;
#4109 = AXIS2_PLACEMENT_3D ( 'NONE', #24073, #16635, #3465 ) ;
#4110 = DIRECTION ( 'NONE',  ( 0.000000000000000000, -0.000000000000000000, -1.000000000000000000 ) ) ;
#4111 = CARTESIAN_POINT ( 'NONE',  ( 83.60204634018053582, -9.244463733058732095E-30, 5.000000000000007994 ) ) ;
#4112 = AXIS2_PLACEMENT_3D ( 'NONE', #20625, #11447, #18925 ) ;
#4113 = CARTESIAN_POINT ( 'NONE',  ( 77.78386452199872281, -5.000000000000009770, 0.000000000000000000 ) ) ;
#4114 = CIRCLE ( 'NONE', #6510, 5.000000000000007994 ) ;
#4115 = LINE ( 'NONE', #20951, #13285 ) ;
#4116 = FACE_OUTER_BOUND ( 'NONE', #6757, .T. ) ;
#4117 = CARTESIAN_POINT ( 'NONE',  ( 15.78970982176773674, 5.581464347350856059, -7.700125654604351055 ) ) ;
#4118 = CIRCLE ( 'NONE', #3331, 4.249999999999996447 ) ;
#4119 = CIRCLE ( 'NONE', #22431, 21.85000000000000142 ) ;
#4120 = EDGE_CURVE ( 'NONE', #4095, #19404, #2671, .T. ) ;
#4121 = LINE ( 'NONE', #13506, #22018 ) ;
#4122 = DIRECTION ( 'NONE',  ( 0.000000000000000000, -1.000000000000000000, 0.000000000000000000 ) ) ;
#4123 = ORIENTED_EDGE ( 'NONE', *, *, #183, .T. ) ;
#4124 = ORIENTED_EDGE ( 'NONE', *, *, #6793, .T. ) ;
#4125 = EDGE_CURVE ( 'NONE', #13623, #3029, #3828, .T. ) ;
#4126 = ADVANCED_FACE ( 'NONE', ( #12966 ), #13324, .T. ) ;
#4127 = VECTOR ( 'NONE', #18758, 1000.000000000000000 ) ;
#4128 = ORIENTED_EDGE ( 'NONE', *, *, #9507, .F. ) ;
#4129 =( GEOMETRIC_REPRESENTATION_CONTEXT ( 3 ) GLOBAL_UNCERTAINTY_ASSIGNED_CONTEXT ( ( #4741 ) ) GLOBAL_UNIT_ASSIGNED_CONTEXT ( ( #13544, #15859, #12176 ) ) REPRESENTATION_CONTEXT ( 'NONE', 'WORKASPACE' ) );
#4130 = AXIS2_PLACEMENT_3D ( 'NONE', #9706, #9465, #234 ) ;
#4131 = VERTEX_POINT ( 'NONE', #9764 ) ;
#4132 = CARTESIAN_POINT ( 'NONE',  ( 0.000000000000000000, -45.00000000000000000, 27.00000000000000000 ) ) ;
#4133 = CARTESIAN_POINT ( 'NONE',  ( 7.685661446562381371, -5.583959896777971110, 9.859589141758144493 ) ) ;
#4134 = AXIS2_PLACEMENT_3D ( 'NONE', #7989, #15437, #6175 ) ;
#4135 = AXIS2_PLACEMENT_3D ( 'NONE', #11872, #7830, #9917 ) ;
#4136 = DIRECTION ( 'NONE',  ( 0.000000000000000000, -1.000000000000000000, 0.000000000000000000 ) ) ;
#4137 = DIRECTION ( 'NONE',  ( 0.000000000000000000, -1.000000000000000000, 0.000000000000000000 ) ) ;
#4138 = FACE_OUTER_BOUND ( 'NONE', #6749, .T. ) ;
#4139 = CARTESIAN_POINT ( 'NONE',  ( 0.000000000000000000, -15.03999999999999915, 27.00000000000000000 ) ) ;
#4140 = EDGE_LOOP ( 'NONE', ( #15511, #20628, #22661, #4038, #23237 ) ) ;
#4141 = ORIENTED_EDGE ( 'NONE', *, *, #1211, .T. ) ;
#4142 = CARTESIAN_POINT ( 'NONE',  ( -36.00000000000000711, -51.00000000000000711, 12.50000000000000000 ) ) ;
#4143 = DIRECTION ( 'NONE',  ( 0.000000000000000000, 0.000000000000000000, 1.000000000000000000 ) ) ;
#4144 = ORIENTED_EDGE ( 'NONE', *, *, #5812, .T. ) ;
#4145 = AXIS2_PLACEMENT_3D ( 'NONE', #4989, #1670, #23871 ) ;
#4146 =( NAMED_UNIT ( * ) PLANE_ANGLE_UNIT ( ) SI_UNIT ( $, .RADIAN. ) );
#4147 = CYLINDRICAL_SURFACE ( 'NONE', #19590, 9.000000000000000000 ) ;
#4148 = CYLINDRICAL_SURFACE ( 'NONE', #2837, 4.249999999999996447 ) ;
#4149 = AXIS2_PLACEMENT_3D ( 'NONE', #823, #8236, #6443 ) ;
#4150 = EDGE_CURVE ( 'NONE', #23011, #12230, #6019, .T. ) ;
#4151 = VECTOR ( 'NONE', #9293, 1000.000000000000000 ) ;
#4152 = PLANE ( 'NONE',  #12609 ) ;
#4153 = ORIENTED_EDGE ( 'NONE', *, *, #23419, .F. ) ;
#4154 = CARTESIAN_POINT ( 'NONE',  ( -8.680847955710813579, -2.820578480814258437, -7.733165578109187699 ) ) ;
#4155 = CARTESIAN_POINT ( 'NONE',  ( -37.00000000000000711, 29.49999999999999645, 12.00000000000000000 ) ) ;
#4156 = AXIS2_PLACEMENT_3D ( 'NONE', #15889, #6373, #2712 ) ;
#4157 = EDGE_CURVE ( 'NONE', #208, #23418, #20660, .T. ) ;
#4158 = ORIENTED_EDGE ( 'NONE', *, *, #8594, .F. ) ;
#4159 = VERTEX_POINT ( 'NONE', #5670 ) ;
#4160 = CARTESIAN_POINT ( 'NONE',  ( 9.500000000000000000, 6.470877716354879437E-13, 8.059589141758143782 ) ) ;
#4161 = EDGE_CURVE ( 'NONE', #13291, #8450, #19829, .T. ) ;
#4162 = ORIENTED_EDGE ( 'NONE', *, *, #5391, .T. ) ;
#4163 = EDGE_CURVE ( 'NONE', #17900, #11505, #21773, .T. ) ;
#4164 = FACE_OUTER_BOUND ( 'NONE', #199, .T. ) ;
#4165 = DIRECTION ( 'NONE',  ( 1.000000000000000000, 1.224606353822377258E-16, 0.000000000000000000 ) ) ;
#4166 = DIRECTION ( 'NONE',  ( 1.000000000000000000, 0.000000000000000000, 0.000000000000000000 ) ) ;
#4167 = DIRECTION ( 'NONE',  ( -1.000000000000000000, -1.224606353822377258E-16, -0.000000000000000000 ) ) ;
#4168 = AXIS2_PLACEMENT_3D ( 'NONE', #3706, #3571, #2107 ) ;
#4169 = DIRECTION ( 'NONE',  ( -1.000000000000000000, -1.224606353822377258E-16, -0.000000000000000000 ) ) ;
#4170 = FACE_OUTER_BOUND ( 'NONE', #4572, .T. ) ;
#4171 = AXIS2_PLACEMENT_3D ( 'NONE', #17553, #10476, #23552 ) ;
#4172 = CARTESIAN_POINT ( 'NONE',  ( -9.499999999999790390, -3.086737114213257804, -3.159589141758143871 ) ) ;
#4173 = VERTEX_POINT ( 'NONE', #20555 ) ;
#4174 = FACE_OUTER_BOUND ( 'NONE', #21746, .T. ) ;
#4175 = ADVANCED_FACE ( 'NONE', ( #4076 ), #16690, .F. ) ;
#4176 = EDGE_LOOP ( 'NONE', ( #23806, #10276, #657, #4956 ) ) ;
#4177 = DIRECTION ( 'NONE',  ( 0.000000000000000000, 0.000000000000000000, 1.000000000000000000 ) ) ;
#4178 = CARTESIAN_POINT ( 'NONE',  ( 0.9720249034408605660, 8.949203418382943198, 78.15512200942710308 ) ) ;
#4179 = FILL_AREA_STYLE ('',( #2586 ) ) ;
#4180 = DIRECTION ( 'NONE',  ( 1.000000000000000000, 2.600433232233976523E-16, -0.000000000000000000 ) ) ;
#4181 = ADVANCED_FACE ( 'NONE', ( #3827 ), #11236, .T. ) ;
#4182 = CARTESIAN_POINT ( 'NONE',  ( 9.324366623732823450E-16, 6.000000000000000000, 80.99999999999998579 ) ) ;
#4183 = AXIS2_PLACEMENT_3D ( 'NONE', #6242, #21126, #2828 ) ;
#4184 = DIRECTION ( 'NONE',  ( -0.000000000000000000, -1.000000000000000000, -0.000000000000000000 ) ) ;
#4185 = DIRECTION ( 'NONE',  ( 0.000000000000000000, 0.000000000000000000, 1.000000000000000000 ) ) ;
#4186 = DIRECTION ( 'NONE',  ( 1.000000000000000000, -2.600433232233976523E-16, -0.000000000000000000 ) ) ;
#4187 = EDGE_LOOP ( 'NONE', ( #19519, #7340, #15155, #7051, #4359, #19941 ) ) ;
#4188 = CARTESIAN_POINT ( 'NONE',  ( -31.74999999999995737, 0.000000000000000000, 5.000000000000000888 ) ) ;
#4189 = ADVANCED_FACE ( 'NONE', ( #12087 ), #5374, .F. ) ;
#4190 = CARTESIAN_POINT ( 'NONE',  ( -2.682529543899159208, -8.255977015246598327, 8.033165578109189298 ) ) ;
#4191 = ADVANCED_FACE ( 'NONE', ( #19561 ), #896, .T. ) ;
#4192 = DIRECTION ( 'NONE',  ( -0.000000000000000000, -0.000000000000000000, -1.000000000000000000 ) ) ;
#4193 = ORIENTED_EDGE ( 'NONE', *, *, #6657, .F. ) ;
#4194 = VERTEX_POINT ( 'NONE', #21025 ) ;
#4195 = DIRECTION ( 'NONE',  ( -1.000000000000000000, -1.224606353822377258E-16, -0.000000000000000000 ) ) ;
#4196 = CARTESIAN_POINT ( 'NONE',  ( 9.500000000000000000, 6.470877716354879437E-13, -9.206742014460234103 ) ) ;
#4197 = VERTEX_POINT ( 'NONE', #13692 ) ;
#4198 = EDGE_CURVE ( 'NONE', #18108, #4194, #10019, .T. ) ;
#4199 = CARTESIAN_POINT ( 'NONE',  ( -30.44534269664590198, -40.40463133211081015, 27.00000000000000000 ) ) ;
#4200 = EDGE_LOOP ( 'NONE', ( #18193, #22903, #19023, #3515, #14629, #810 ) ) ;
#4201 = ADVANCED_FACE ( 'NONE', ( #15900 ), #9901, .F. ) ;
#4202 = EDGE_LOOP ( 'NONE', ( #14797, #11093 ) ) ;
#4203 = DIRECTION ( 'NONE',  ( 0.000000000000000000, 1.000000000000000000, 0.000000000000000000 ) ) ;
#4204 = FACE_BOUND ( 'NONE', #16851, .T. ) ;
#4205 = DIRECTION ( 'NONE',  ( 0.000000000000000000, 0.000000000000000000, 1.000000000000000000 ) ) ;
#4206 = CARTESIAN_POINT ( 'NONE',  ( 23.90000000000000568, 29.50000000000000355, 12.00000000000000000 ) ) ;
#4207 = VERTEX_POINT ( 'NONE', #662 ) ;
#4208 = CARTESIAN_POINT ( 'NONE',  ( -23.85000000000000142, 15.03999999999999737, 2.200000000000000178 ) ) ;
#4209 = DIRECTION ( 'NONE',  ( -1.000000000000000000, 0.000000000000000000, 0.000000000000000000 ) ) ;
#4210 = ORIENTED_EDGE ( 'NONE', *, *, #7673, .T. ) ;
#4211 = ORIENTED_EDGE ( 'NONE', *, *, #4125, .F. ) ;
#4212 = CARTESIAN_POINT ( 'NONE',  ( -7.022953521755574080, 5.102474405759713783, 7.433165578109188765 ) ) ;
#4213 = AXIS2_PLACEMENT_3D ( 'NONE', #14067, #4814, #21400 ) ;
#4214 = ORIENTED_EDGE ( 'NONE', *, *, #10870, .F. ) ;
#4215 = VERTEX_POINT ( 'NONE', #12224 ) ;
#4216 = DIRECTION ( 'NONE',  ( -1.000000000000000000, 0.000000000000000000, 0.000000000000000000 ) ) ;
#4217 = ORIENTED_EDGE ( 'NONE', *, *, #14565, .T. ) ;
#4218 = ORIENTED_EDGE ( 'NONE', *, *, #15134, .F. ) ;
#4219 = CARTESIAN_POINT ( 'NONE',  ( 5.000000000000000000, 3.513898075855357295, -2.028750000000005382 ) ) ;
#4220 = CARTESIAN_POINT ( 'NONE',  ( 8.680847955711199049, -2.820578480813074496, -4.533165578109188409 ) ) ;
#4221 = PRODUCT_RELATED_PRODUCT_CATEGORY ( 'part', '', ( #21328 ) ) ;
#4222 = FACE_OUTER_BOUND ( 'NONE', #14254, .T. ) ;
#4223 = ORIENTED_EDGE ( 'NONE', *, *, #2826, .F. ) ;
#4224 = DIRECTION ( 'NONE',  ( 0.000000000000000000, 1.000000000000000000, 0.000000000000000000 ) ) ;
#4225 = LINE ( 'NONE', #6054, #13883 ) ;
#4226 = DIRECTION ( 'NONE',  ( 0.000000000000000000, 0.000000000000000000, 1.000000000000000000 ) ) ;
#4227 = DIRECTION ( 'NONE',  ( -1.000000000000000000, 0.000000000000000000, 0.000000000000000000 ) ) ;
#4228 = DIRECTION ( 'NONE',  ( -1.000000000000000000, -1.224606353822377258E-16, -0.000000000000000000 ) ) ;
#4229 = CARTESIAN_POINT ( 'NONE',  ( 31.10231664966676135, 45.36128193761570770, -27.00000000000000000 ) ) ;
#4230 = EDGE_CURVE ( 'NONE', #23824, #18698, #23099, .T. ) ;
#4231 = EDGE_CURVE ( 'NONE', #15166, #5560, #11284, .T. ) ;
#4232 = ORIENTED_EDGE ( 'NONE', *, *, #14831, .T. ) ;
#4233 = CARTESIAN_POINT ( 'NONE',  ( -41.00000000000000000, 4.000000000000000888, 9.500000000000000000 ) ) ;
#4234 = CARTESIAN_POINT ( 'NONE',  ( 9.500000000000000000, 6.470877716354879437E-13, -8.059589141758143782 ) ) ;
#4235 = CARTESIAN_POINT ( 'NONE',  ( -30.44534269664590198, 40.40463133211079594, -27.00000000000000000 ) ) ;
#4236 = FACE_OUTER_BOUND ( 'NONE', #23387, .T. ) ;
#4237 = DIRECTION ( 'NONE',  ( 0.000000000000000000, 0.000000000000000000, -1.000000000000000000 ) ) ;
#4238 = CARTESIAN_POINT ( 'NONE',  ( -8.680847955711200825, 2.820578480813073607, -9.533165578109189298 ) ) ;
#4239 = CONICAL_SURFACE ( 'NONE', #19482, 4.172000000000008590, 0.9599310885968742602 ) ;
#4240 = CARTESIAN_POINT ( 'NONE',  ( -7.685661446561619314, -5.583959896779019161, 8.406742014460233392 ) ) ;
#4241 = VERTEX_POINT ( 'NONE', #4313 ) ;
#4242 = EDGE_LOOP ( 'NONE', ( #18336, #20675, #7375, #13202 ) ) ;
#4243 = CARTESIAN_POINT ( 'NONE',  ( -2.682529543900285862, 8.255977015246234174, 11.23316557810918859 ) ) ;
#4244 = VERTEX_POINT ( 'NONE', #21139 ) ;
#4245 = DIRECTION ( 'NONE',  ( 8.118380936277290665E-16, 1.793782002643211550E-15, -0.9999999999999998890 ) ) ;
#4246 = CARTESIAN_POINT ( 'NONE',  ( -23.84999999999999432, -15.03999999999999915, 25.00000000000000000 ) ) ;
#4247 = ORIENTED_EDGE ( 'NONE', *, *, #18637, .F. ) ;
#4248 = DIRECTION ( 'NONE',  ( -1.000000000000000000, -0.000000000000000000, -0.000000000000000000 ) ) ;
#4249 = CARTESIAN_POINT ( 'NONE',  ( 2.935661446561383503, 9.035036904804158553, -10.45958914175814414 ) ) ;
#4250 = PRODUCT_DEFINITION_CONTEXT ( 'detailed design', #22721, 'design' ) ;
#4251 = EDGE_CURVE ( 'NONE', #13101, #14561, #12474, .T. ) ;
#4252 = FACE_OUTER_BOUND ( 'NONE', #4086, .T. ) ;
#4253 = LINE ( 'NONE', #5834, #20104 ) ;
#4254 = CARTESIAN_POINT ( 'NONE',  ( -9.500000000000000000, -6.482511860946779655E-13, 6.206742014460234103 ) ) ;
#4255 = CIRCLE ( 'NONE', #1164, 6.050000000006050982 ) ;
#4256 = ORIENTED_EDGE ( 'NONE', *, *, #3072, .F. ) ;
#4257 = CARTESIAN_POINT ( 'NONE',  ( -28.99999999999999645, -29.50000000000001066, 27.00000000000000000 ) ) ;
#4258 = ADVANCED_FACE ( 'NONE', ( #1031, #2975, #23359, #17227, #8184, #6389 ), #17362, .T. ) ;
#4259 = CARTESIAN_POINT ( 'NONE',  ( 74.57977184163763695, 7.562528597612068045E-15, 0.000000000000000000 ) ) ;
#4260 = EDGE_CURVE ( 'NONE', #15663, #13780, #10089, .T. ) ;
#4261 = CARTESIAN_POINT ( 'NONE',  ( 0.9999999999999986677, 0.000000000000000000, 11.22592346138681130 ) ) ;
#4262 = EDGE_CURVE ( 'NONE', #20648, #18900, #15775, .T. ) ;
#4263 = ORIENTED_EDGE ( 'NONE', *, *, #787, .T. ) ;
#4264 = DIRECTION ( 'NONE',  ( 0.000000000000000000, -1.000000000000000000, 0.000000000000000000 ) ) ;
#4265 = DIRECTION ( 'NONE',  ( 0.000000000000000000, 0.000000000000000000, 1.000000000000000000 ) ) ;
#4266 = EDGE_CURVE ( 'NONE', #760, #11663, #3661, .T. ) ;
#4267 = DIRECTION ( 'NONE',  ( -0.000000000000000000, -0.000000000000000000, -1.000000000000000000 ) ) ;
#4268 = LINE ( 'NONE', #19140, #16912 ) ;
#4269 = ORIENTED_EDGE ( 'NONE', *, *, #18401, .T. ) ;
#4270 = CARTESIAN_POINT ( 'NONE',  ( -2.682529543900285862, 8.255977015246234174, -7.233165578109188587 ) ) ;
#4271 = VERTEX_POINT ( 'NONE', #15516 ) ;
#4272 = VERTEX_POINT ( 'NONE', #6252 ) ;
#4273 = CARTESIAN_POINT ( 'NONE',  ( 2.935661446561383503, 9.035036904804158553, 10.45958914175814414 ) ) ;
#4274 = CARTESIAN_POINT ( 'NONE',  ( 7.685661446561619314, 5.583959896779020049, 11.40674201446023517 ) ) ;
#4275 = ORIENTED_EDGE ( 'NONE', *, *, #22723, .F. ) ;
#4276 = DIRECTION ( 'NONE',  ( 0.000000000000000000, 0.000000000000000000, 1.000000000000000000 ) ) ;
#4277 = DIRECTION ( 'NONE',  ( 0.000000000000000000, 1.000000000000000000, 0.000000000000000000 ) ) ;
#4278 = VECTOR ( 'NONE', #7924, 1000.000000000000000 ) ;
#4279 = FACE_OUTER_BOUND ( 'NONE', #1390, .T. ) ;
#4280 = FACE_OUTER_BOUND ( 'NONE', #21379, .T. ) ;
#4281 = ADVANCED_FACE ( 'NONE', ( #2611, #17476 ), #4571, .F. ) ;
#4282 = DIRECTION ( 'NONE',  ( -1.000000000000000000, -0.000000000000000000, -0.000000000000000000 ) ) ;
#4283 = DIRECTION ( 'NONE',  ( -0.000000000000000000, -0.000000000000000000, 1.000000000000000000 ) ) ;
#4284 = CARTESIAN_POINT ( 'NONE',  ( 74.57977184163763695, 7.562528597612068045E-15, 0.000000000000000000 ) ) ;
#4285 = ORIENTED_EDGE ( 'NONE', *, *, #19789, .F. ) ;
#4286 = CARTESIAN_POINT ( 'NONE',  ( 76.03431729618309021, 7.562528597612068045E-15, 0.000000000000000000 ) ) ;
#4287 = EDGE_CURVE ( 'NONE', #1878, #18602, #10136, .T. ) ;
#4288 = EDGE_CURVE ( 'NONE', #7451, #21069, #559, .T. ) ;
#4289 = EDGE_LOOP ( 'NONE', ( #23694, #11628, #21620, #16111, #7306, #4275 ) ) ;
#4290 = CARTESIAN_POINT ( 'NONE',  ( 3.586653933227395008, -8.272513638839596339, 12.49187530341550278 ) ) ;
#4291 = AXIS2_PLACEMENT_3D ( 'NONE', #17648, #711, #952 ) ;
#4292 = CARTESIAN_POINT ( 'NONE',  ( -9.210377633962220756, 2.035213337404456535, 12.08117117427555165 ) ) ;
#4293 = CARTESIAN_POINT ( 'NONE',  ( 62.36363636363636687, 4.172000000000015696, 5.109226446042767468E-16 ) ) ;
#4294 = VECTOR ( 'NONE', #867, 1000.000000000000000 ) ;
#4295 = CARTESIAN_POINT ( 'NONE',  ( -31.74999999999995737, 0.000000000000000000, 5.000000000000000888 ) ) ;
#4296 = LINE ( 'NONE', #9878, #351 ) ;
#4297 = LINE ( 'NONE', #19425, #3600 ) ;
#4298 = FACE_OUTER_BOUND ( 'NONE', #12334, .T. ) ;
#4299 = CARTESIAN_POINT ( 'NONE',  ( -5.871322893123450015, -8.081182679344781405, -6.506742014460233925 ) ) ;
#4300 = ORIENTED_EDGE ( 'NONE', *, *, #10786, .F. ) ;
#4301 = DIRECTION ( 'NONE',  ( -0.000000000000000000, 0.000000000000000000, 1.000000000000000000 ) ) ;
#4302 = CARTESIAN_POINT ( 'NONE',  ( -8.680847955711200825, 2.820578480813073607, 11.53316557810918752 ) ) ;
#4303 = CARTESIAN_POINT ( 'NONE',  ( 9.000000000000000000, 1.102182119232617714E-15, 15.50000000000000000 ) ) ;
#4304 = DIRECTION ( 'NONE',  ( 0.000000000000000000, 0.000000000000000000, -1.000000000000000000 ) ) ;
#4305 = CARTESIAN_POINT ( 'NONE',  ( 4.029965094393306726E-41, -5.916456789157588541E-28, 21.50000000000009592 ) ) ;
#4306 = ORIENTED_EDGE ( 'NONE', *, *, #11333, .T. ) ;
#4307 = ITEM_DEFINED_TRANSFORMATION ( 'NONE', 'NONE', #13466,  #8005 ) ;
#4308 = ORIENTED_EDGE ( 'NONE', *, *, #22916, .T. ) ;
#4309 = CARTESIAN_POINT ( 'NONE',  ( 40.00000000000000711, 15.50000000000000533, 12.50000000000000000 ) ) ;
#4310 = CARTESIAN_POINT ( 'NONE',  ( 7.685661446562381371, -5.583959896777971110, -9.006742014460233037 ) ) ;
#4311 = ORIENTED_EDGE ( 'NONE', *, *, #2396, .T. ) ;
#4312 = ADVANCED_FACE ( 'NONE', ( #5917 ), #23149, .T. ) ;
#4313 = CARTESIAN_POINT ( 'NONE',  ( -40.77574956473004164, -27.49633847812775755, 11.00000000000000000 ) ) ;
#4314 = ORIENTED_EDGE ( 'NONE', *, *, #1104, .F. ) ;
#4315 = CARTESIAN_POINT ( 'NONE',  ( -9.499999952843596773, -0.5398784843733258620, -3.499626879768900523 ) ) ;
#4316 = ORIENTED_EDGE ( 'NONE', *, *, #19214, .F. ) ;
#4317 = CARTESIAN_POINT ( 'NONE',  ( -18.49999999999999645, -15.23000000000000220, 27.00000000000000000 ) ) ;
#4318 = CARTESIAN_POINT ( 'NONE',  ( 41.73082370883260239, 29.49999999999999645, 0.000000000000000000 ) ) ;
#4319 = PRODUCT_DEFINITION_CONTEXT ( 'detailed design', #20101, 'design' ) ;
#4320 = CARTESIAN_POINT ( 'NONE',  ( 61.48886275072855057, 5.000000000000015987, 0.000000000000000000 ) ) ;
#4321 = AXIS2_PLACEMENT_3D ( 'NONE', #15939, #23402, #6672 ) ;
#4322 = ORIENTED_EDGE ( 'NONE', *, *, #11637, .T. ) ;
#4323 = FACE_OUTER_BOUND ( 'NONE', #21327, .T. ) ;
#4324 = CARTESIAN_POINT ( 'NONE',  ( 42.00000000000000000, 26.82133436441678853, 0.000000000000000000 ) ) ;
#4325 = CARTESIAN_POINT ( 'NONE',  ( -31.50000000000000711, -51.00000000000000711, 0.5000000000000004441 ) ) ;
#4326 = ORIENTED_EDGE ( 'NONE', *, *, #6800, .F. ) ;
#4327 = EDGE_LOOP ( 'NONE', ( #17196, #7757, #8235, #17359, #9739 ) ) ;
#4328 = CARTESIAN_POINT ( 'NONE',  ( 5.871322893124553133, -8.081182679343980269, 7.759589141758143072 ) ) ;
#4329 = VERTEX_POINT ( 'NONE', #2011 ) ;
#4330 = EDGE_LOOP ( 'NONE', ( #20573, #13953, #2591, #20472, #14083 ) ) ;
#4331 = ADVANCED_FACE ( 'NONE', ( #7980, #4222 ), #20449, .T. ) ;
#4332 = ORIENTED_EDGE ( 'NONE', *, *, #20597, .T. ) ;
#4333 = ORIENTED_EDGE ( 'NONE', *, *, #12912, .F. ) ;
#4334 = EDGE_CURVE ( 'NONE', #9132, #5402, #6788, .T. ) ;
#4335 = DIRECTION ( 'NONE',  ( 0.000000000000000000, 1.000000000000000000, 0.000000000000000000 ) ) ;
#4336 = CARTESIAN_POINT ( 'NONE',  ( 7.022953521755574080, -5.102474405759714671, -4.433165578109187877 ) ) ;
#4337 = CARTESIAN_POINT ( 'NONE',  ( 7.685661446561619314, 5.583959896779020049, 7.406742014460233392 ) ) ;
#4338 = EDGE_CURVE ( 'NONE', #21201, #1469, #12599, .T. ) ;
#4339 = AXIS2_PLACEMENT_3D ( 'NONE', #12061, #19793, #21370 ) ;
#4340 = ORIENTED_EDGE ( 'NONE', *, *, #5537, .F. ) ;
#4341 = DIRECTION ( 'NONE',  ( -0.000000000000000000, -0.000000000000000000, 1.000000000000000000 ) ) ;
#4342 = DIRECTION ( 'NONE',  ( 0.7071067811865474617, 8.659560562354932858E-17, -0.7071067811865474617 ) ) ;
#4344 = DIRECTION ( 'NONE',  ( -1.000000000000000000, -0.000000000000000000, -0.000000000000000000 ) ) ;
#4343 =( REPRESENTATION_RELATIONSHIP ('NONE','NONE', #21748, #15290 ) REPRESENTATION_RELATIONSHIP_WITH_TRANSFORMATION ( #48 )SHAPE_REPRESENTATION_RELATIONSHIP( ) );
#4345 = EDGE_CURVE ( 'NONE', #15317, #2103, #5213, .T. ) ;
#4346 = DIRECTION ( 'NONE',  ( 0.000000000000000000, 0.000000000000000000, 1.000000000000000000 ) ) ;
#4347 = FACE_OUTER_BOUND ( 'NONE', #11169, .T. ) ;
#4348 = PRESENTATION_LAYER_ASSIGNMENT (  '', '', ( #2793 ) ) ;
#4349 = ORIENTED_EDGE ( 'NONE', *, *, #14997, .T. ) ;
#4350 = CYLINDRICAL_SURFACE ( 'NONE', #23233, 1.500000000000000000 ) ;
#4351 = DIRECTION ( 'NONE',  ( -0.000000000000000000, -0.000000000000000000, -1.000000000000000000 ) ) ;
#4352 = ORIENTED_EDGE ( 'NONE', *, *, #20070, .F. ) ;
#4353 = CARTESIAN_POINT ( 'NONE',  ( -1.749335460929532182, -9.337549220493269075, 3.500000000000028866 ) ) ;
#4354 = CARTESIAN_POINT ( 'NONE',  ( -40.23082370883260239, 29.50000000000000711, -3.000000000000000000 ) ) ;
#4355 = CARTESIAN_POINT ( 'NONE',  ( 60.03431729618309021, -5.000000000000000888, 6.123233995736776143E-16 ) ) ;
#4356 = CARTESIAN_POINT ( 'NONE',  ( -9.500000000000000000, -6.482511860946779655E-13, 5.059589141758143782 ) ) ;
#4357 = CARTESIAN_POINT ( 'NONE',  ( -5.365059087799948223, 7.384370330706355290, -7.333165578109188232 ) ) ;
#4358 = ORIENTED_EDGE ( 'NONE', *, *, #18640, .F. ) ;
#4359 = ORIENTED_EDGE ( 'NONE', *, *, #3675, .T. ) ;
#4360 = ORIENTED_EDGE ( 'NONE', *, *, #10513, .F. ) ;
#4361 = CARTESIAN_POINT ( 'NONE',  ( -8.680847955710813579, -2.820578480814258437, 7.733165578109187699 ) ) ;
#4362 = AXIS2_PLACEMENT_3D ( 'NONE', #16746, #18246, #1538 ) ;
#4363 = ORIENTED_EDGE ( 'NONE', *, *, #9525, .F. ) ;
#4364 = DIRECTION ( 'NONE',  ( 1.000000000000000000, -6.938893903907228378E-16, 2.775557561562890735E-17 ) ) ;
#4365 = DIRECTION ( 'NONE',  ( 0.000000000000000000, 0.000000000000000000, 1.000000000000000000 ) ) ;
#4366 = ADVANCED_FACE ( 'NONE', ( #20941 ), #9435, .F. ) ;
#4367 = LINE ( 'NONE', #713, #18520 ) ;
#4368 = CARTESIAN_POINT ( 'NONE',  ( 35.99999999999992184, -60.00000000000000000, 12.50000000000000000 ) ) ;
#4369 = EDGE_CURVE ( 'NONE', #7962, #16829, #2263, .T. ) ;
#4370 = DIRECTION ( 'NONE',  ( -0.000000000000000000, 1.000000000000000000, 1.224646799147353207E-16 ) ) ;
#4371 = DIRECTION ( 'NONE',  ( 0.000000000000000000, -1.000000000000000000, 0.000000000000000000 ) ) ;
#4372 = DIRECTION ( 'NONE',  ( 0.000000000000000000, -0.000000000000000000, 1.000000000000000000 ) ) ;
#4373 = CARTESIAN_POINT ( 'NONE',  ( 3.000000000000000888, 6.000000000000000000, 80.99999999999998579 ) ) ;
#4374 = DIRECTION ( 'NONE',  ( -2.600433232233976523E-16, -1.000000000000000000, 0.000000000000000000 ) ) ;
#4375 = AXIS2_PLACEMENT_3D ( 'NONE', #331, #20463, #16777 ) ;
#4376 = CONICAL_SURFACE ( 'NONE', #18012, 4.172000000000008590, 0.9599310885968742602 ) ;
#4377 = FACE_OUTER_BOUND ( 'NONE', #21705, .T. ) ;
#4378 = EDGE_LOOP ( 'NONE', ( #20286, #5573, #7676, #8909 ) ) ;
#4379 = DIRECTION ( 'NONE',  ( 0.000000000000000000, 0.000000000000000000, 1.000000000000000000 ) ) ;
#4380 = DIRECTION ( 'NONE',  ( -1.000000000000000000, 0.000000000000000000, 0.000000000000000000 ) ) ;
#4381 = VECTOR ( 'NONE', #8189, 1000.000000000000000 ) ;
#4382 = CARTESIAN_POINT ( 'NONE',  ( 23.00000000000000000, -9.374578970469700678, 10.68280860024311885 ) ) ;
#4383 = CIRCLE ( 'NONE', #9407, 7.999999999999992895 ) ;
#4384 = CONICAL_SURFACE ( 'NONE', #19197, 8.500000000000000000, 0.9519047898634274141 ) ;
#4385 = DIRECTION ( 'NONE',  ( -1.000000000000000000, -0.000000000000000000, -0.000000000000000000 ) ) ;
#4386 = ORIENTED_EDGE ( 'NONE', *, *, #16386, .T. ) ;
#4387 = PRODUCT_RELATED_PRODUCT_CATEGORY ( 'part', '', ( #857 ) ) ;
#4388 = EDGE_CURVE ( 'NONE', #8454, #8991, #20410, .T. ) ;
#4389 = ORIENTED_EDGE ( 'NONE', *, *, #11843, .T. ) ;
#4390 = CARTESIAN_POINT ( 'NONE',  ( 9.500000000000000000, 6.470877716354879437E-13, 10.05958914175814378 ) ) ;
#4391 = CARTESIAN_POINT ( 'NONE',  ( -6.822232771736903637E-13, 9.988891130263535700, 11.70674201446023410 ) ) ;
#4392 = ORIENTED_EDGE ( 'NONE', *, *, #9196, .F. ) ;
#4393 =( NAMED_UNIT ( * ) SI_UNIT ( $, .STERADIAN. ) SOLID_ANGLE_UNIT ( ) );
#4394 = EDGE_CURVE ( 'NONE', #17386, #5961, #22359, .T. ) ;
#4395 = LINE ( 'NONE', #15860, #2104 ) ;
#4396 = DIRECTION ( 'NONE',  ( 1.000000000000000000, 0.000000000000000000, 0.000000000000000000 ) ) ;
#4397 = AXIS2_PLACEMENT_3D ( 'NONE', #18513, #7034, #5455 ) ;
#4398 = EDGE_CURVE ( 'NONE', #2976, #8087, #3967, .T. ) ;
#4399 = VECTOR ( 'NONE', #2226, 1000.000000000000000 ) ;
#4400 = CONICAL_SURFACE ( 'NONE', #13719, 5.000000000000007994, 0.9599310885968855844 ) ;
#4401 = DIRECTION ( 'NONE',  ( -1.000000000000000000, 0.000000000000000000, 9.637352644315592778E-17 ) ) ;
#4402 = ADVANCED_FACE ( 'NONE', ( #15291 ), #20819, .T. ) ;
#4403 = CIRCLE ( 'NONE', #22321, 4.172000000000008590 ) ;
#4404 = VECTOR ( 'NONE', #14729, 1000.000000000000000 ) ;
#4405 = CIRCLE ( 'NONE', #23498, 6.050000000006054535 ) ;
#4406 = CARTESIAN_POINT ( 'NONE',  ( 7.000000000000000888, 0.000000000000000000, 0.000000000000000000 ) ) ;
#4407 = PLANE ( 'NONE',  #7958 ) ;
#4408 = DIRECTION ( 'NONE',  ( 1.000000000000000000, 1.224606353822377258E-16, 0.000000000000000000 ) ) ;
#4409 = AXIS2_PLACEMENT_3D ( 'NONE', #6047, #20939, #17016 ) ;
#4410 = CARTESIAN_POINT ( 'NONE',  ( -9.500000000000211386, 3.086737114211961064, -2.959589141758143249 ) ) ;
#4411 = ORIENTED_EDGE ( 'NONE', *, *, #12173, .T. ) ;
#4412 = ORIENTED_EDGE ( 'NONE', *, *, #4935, .T. ) ;
#4413 = CARTESIAN_POINT ( 'NONE',  ( -4.277975316535544970, -8.125595891023657202, 12.32532379220425867 ) ) ;
#4414 = CARTESIAN_POINT ( 'NONE',  ( 0.000000000000000000, 45.00000000000000000, -3.000000000000000000 ) ) ;
#4415 = CARTESIAN_POINT ( 'NONE',  ( 14.51962751333974389, 3.765689428759031010, -8.721787840009197268 ) ) ;
#4416 = CIRCLE ( 'NONE', #6357, 5.025000000000002132 ) ;
#4417 = CARTESIAN_POINT ( 'NONE',  ( 34.10000000000001563, -29.50000000000000711, -27.00000000000000000 ) ) ;
#4418 = DIRECTION ( 'NONE',  ( -1.000000000000000000, 0.000000000000000000, 0.000000000000000000 ) ) ;
#4419 = CIRCLE ( 'NONE', #7478, 6.050000000006050982 ) ;
#4420 = CARTESIAN_POINT ( 'NONE',  ( 42.00000000000000000, -25.93535998569253920, -27.00000000000000000 ) ) ;
#4421 = AXIS2_PLACEMENT_3D ( 'NONE', #10652, #1172, #10423 ) ;
#4422 = CARTESIAN_POINT ( 'NONE',  ( 41.99999999999999289, 5.618459588085056979E-15, 0.000000000000000000 ) ) ;
#4423 = ORIENTED_EDGE ( 'NONE', *, *, #5043, .F. ) ;
#4424 = ADVANCED_FACE ( 'NONE', ( #17618 ), #689, .T. ) ;
#4425 = CARTESIAN_POINT ( 'NONE',  ( -2.935661446562617183, 9.035036904803758873, -3.806742014460233303 ) ) ;
#4426 = ORIENTED_EDGE ( 'NONE', *, *, #14171, .F. ) ;
#4427 = CARTESIAN_POINT ( 'NONE',  ( -42.00000000000000000, -5.000000000000000888, 11.00000000000000000 ) ) ;
#4428 = CARTESIAN_POINT ( 'NONE',  ( 6.222797240145152671E-13, -9.127583699786111282, 6.133165578109188054 ) ) ;
#4429 = CIRCLE ( 'NONE', #21590, 5.000000000000007994 ) ;
#4430 = CARTESIAN_POINT ( 'NONE',  ( 63.81818181818181301, 4.172000000000015696, 0.000000000000000000 ) ) ;
#4431 = EDGE_CURVE ( 'NONE', #4471, #7020, #14177, .T. ) ;
#4432 = EDGE_CURVE ( 'NONE', #1630, #5584, #7193, .T. ) ;
#4433 = EDGE_LOOP ( 'NONE', ( #1752, #5488, #9441, #5759, #21821 ) ) ;
#4434 = CONTEXT_DEPENDENT_SHAPE_REPRESENTATION ( #1707, #16662 ) ;
#4435 = ORIENTED_EDGE ( 'NONE', *, *, #5691, .F. ) ;
#4436 = DIRECTION ( 'NONE',  ( 0.000000000000000000, -0.000000000000000000, -1.000000000000000000 ) ) ;
#4437 = CIRCLE ( 'NONE', #22752, 5.000000000000007994 ) ;
#4438 = AXIS2_PLACEMENT_3D ( 'NONE', #16653, #16876, #7470 ) ;
#4439 = CARTESIAN_POINT ( 'NONE',  ( -2.935661446562617183, 9.035036904803758873, -11.80674201446023375 ) ) ;
#4440 = ORIENTED_EDGE ( 'NONE', *, *, #21279, .F. ) ;
#4441 = AXIS2_PLACEMENT_3D ( 'NONE', #9929, #12250, #8209 ) ;
#4442 = ORIENTED_EDGE ( 'NONE', *, *, #15884, .T. ) ;
#4443 = CARTESIAN_POINT ( 'NONE',  ( -2.024999999999999911, -45.00000000000000000, -27.00000000000000000 ) ) ;
#4444 = AXIS2_PLACEMENT_3D ( 'NONE', #16497, #14306, #19707 ) ;
#4445 = AXIS2_PLACEMENT_3D ( 'NONE', #193, #11247, #20672 ) ;
#4446 = DIRECTION ( 'NONE',  ( -0.000000000000000000, -0.000000000000000000, -1.000000000000000000 ) ) ;
#4447 = CONICAL_SURFACE ( 'NONE', #18084, 4.057500000000000107, 1.047197551196593857 ) ;
#4448 = ORIENTED_EDGE ( 'NONE', *, *, #3556, .F. ) ;
#4449 = ORIENTED_EDGE ( 'NONE', *, *, #9092, .T. ) ;
#4450 = FACE_OUTER_BOUND ( 'NONE', #6189, .T. ) ;
#4451 = CARTESIAN_POINT ( 'NONE',  ( -44.00000000000001421, 50.99999999999999289, 0.5000000000000000000 ) ) ;
#4452 = DIRECTION ( 'NONE',  ( -1.000000000000000000, -0.000000000000000000, -0.000000000000000000 ) ) ;
#4453 = CARTESIAN_POINT ( 'NONE',  ( 23.00000000000000000, 0.000000000000000000, 0.000000000000000000 ) ) ;
#4454 = ORIENTED_EDGE ( 'NONE', *, *, #15224, .T. ) ;
#4455 = PLANE ( 'NONE',  #17294 ) ;
#4456 = CARTESIAN_POINT ( 'NONE',  ( -9.500000000000000000, -6.482511860946779655E-13, 10.20674201446023233 ) ) ;
#4457 = ORIENTED_EDGE ( 'NONE', *, *, #17541, .F. ) ;
#4458 = AXIS2_PLACEMENT_3D ( 'NONE', #16971, #16726, #9518 ) ;
#4459 = VERTEX_POINT ( 'NONE', #21418 ) ;
#4460 = CARTESIAN_POINT ( 'NONE',  ( -9.500000000000211386, 3.086737114211961064, 4.959589141758145026 ) ) ;
#4461 = ORIENTED_EDGE ( 'NONE', *, *, #3814, .T. ) ;
#4462 = AXIS2_PLACEMENT_3D ( 'NONE', #17217, #765, #15617 ) ;
#4463 = ORIENTED_EDGE ( 'NONE', *, *, #1025, .T. ) ;
#4464 = ORIENTED_EDGE ( 'NONE', *, *, #22221, .F. ) ;
#4465 = EDGE_CURVE ( 'NONE', #12301, #2256, #12984, .T. ) ;
#4466 = CONICAL_SURFACE ( 'NONE', #7183, 4.172000000000008590, 0.9599310885968742602 ) ;
#4467 = EDGE_CURVE ( 'NONE', #7243, #8454, #18849, .T. ) ;
#4468 = AXIS2_PLACEMENT_3D ( 'NONE', #839, #14248, #4638 ) ;
#4469 = ORIENTED_EDGE ( 'NONE', *, *, #443, .F. ) ;
#4470 = VERTEX_POINT ( 'NONE', #15801 ) ;
#4471 = VERTEX_POINT ( 'NONE', #21305 ) ;
#4472 = DIRECTION ( 'NONE',  ( -1.000000000000000000, -1.224606353822377258E-16, -0.000000000000000000 ) ) ;
#4473 = CARTESIAN_POINT ( 'NONE',  ( -8.680847955711007202, -5.923547351154968927E-13, -5.633165578109188942 ) ) ;
#4474 = ORIENTED_EDGE ( 'NONE', *, *, #8144, .T. ) ;
#4475 = DIRECTION ( 'NONE',  ( 0.000000000000000000, -1.000000000000000000, 0.000000000000000000 ) ) ;
#4476 = CARTESIAN_POINT ( 'NONE',  ( 83.60204634018053582, 7.420530141404717394E-15, 0.000000000000000000 ) ) ;
#4477 = DIRECTION ( 'NONE',  ( 0.000000000000000000, 0.000000000000000000, -1.000000000000000000 ) ) ;
#4478 = DIRECTION ( 'NONE',  ( -1.000000000000000000, 0.000000000000000000, 0.000000000000000000 ) ) ;
#4479 = DIRECTION ( 'NONE',  ( -1.000000000000000000, -0.000000000000000000, -0.000000000000000000 ) ) ;
#4480 = ORIENTED_EDGE ( 'NONE', *, *, #14219, .T. ) ;
#4481 = CARTESIAN_POINT ( 'NONE',  ( -41.99999999999999289, 0.000000000000000000, 0.000000000000000000 ) ) ;
#4482 = FACE_OUTER_BOUND ( 'NONE', #9215, .T. ) ;
#4483 = CIRCLE ( 'NONE', #18114, 1.499999999999994449 ) ;
#4484 = AXIS2_PLACEMENT_3D ( 'NONE', #11306, #16593, #23925 ) ;
#4485 = EDGE_CURVE ( 'NONE', #17850, #9263, #7923, .T. ) ;
#4486 = ORIENTED_EDGE ( 'NONE', *, *, #2232, .F. ) ;
#4487 = DIRECTION ( 'NONE',  ( -1.000000000000000000, -2.600433232233976523E-16, -0.000000000000000000 ) ) ;
#4488 = DIRECTION ( 'NONE',  ( -1.000000000000000000, -1.224606353822377258E-16, -0.000000000000000000 ) ) ;
#4489 = AXIS2_PLACEMENT_3D ( 'NONE', #19264, #17423, #722 ) ;
#4490 = CARTESIAN_POINT ( 'NONE',  ( 16.82499651802897134, -7.532250541895347595, 5.808290850931478566 ) ) ;
#4491 = AXIS2_PLACEMENT_3D ( 'NONE', #8874, #1685, #14832 ) ;
#4492 = CARTESIAN_POINT ( 'NONE',  ( 41.73082370883257397, 50.99999999999999289, 0.000000000000000000 ) ) ;
#4493 = EDGE_CURVE ( 'NONE', #13963, #9227, #9893, .T. ) ;
#4494 = CARTESIAN_POINT ( 'NONE',  ( 5.365059087798939252, 7.384370330707087149, -10.93316557810918965 ) ) ;
#4495 = VERTEX_POINT ( 'NONE', #21047 ) ;
#4496 = CIRCLE ( 'NONE', #6042, 0.9999999999999991118 ) ;
#4497 = FACE_OUTER_BOUND ( 'NONE', #17667, .T. ) ;
#4498 = ORIENTED_EDGE ( 'NONE', *, *, #17594, .F. ) ;
#4499 = ORIENTED_EDGE ( 'NONE', *, *, #398, .F. ) ;
#4500 = EDGE_CURVE ( 'NONE', #16347, #22742, #5598, .T. ) ;
#4501 = CARTESIAN_POINT ( 'NONE',  ( 7.022953521754877748, 5.102474405760673903, 8.833165578109190008 ) ) ;
#4502 = ORIENTED_EDGE ( 'NONE', *, *, #19031, .F. ) ;
#4503 =( NAMED_UNIT ( * ) PLANE_ANGLE_UNIT ( ) SI_UNIT ( $, .RADIAN. ) );
#4504 = VECTOR ( 'NONE', #17370, 1000.000000000000000 ) ;
#4505 = CARTESIAN_POINT ( 'NONE',  ( 9.499999999999790390, 3.086737114213260025, -11.30674201446023197 ) ) ;
#4506 = VERTEX_POINT ( 'NONE', #12111 ) ;
#4507 = APPLICATION_CONTEXT ( 'automotive_design' ) ;
#4508 = DIRECTION ( 'NONE',  ( 1.000000000000000000, 0.000000000000000000, 0.000000000000000000 ) ) ;
#4509 = DIRECTION ( 'NONE',  ( -0.000000000000000000, -0.000000000000000000, 1.000000000000000000 ) ) ;
#4510 = CIRCLE ( 'NONE', #18893, 5.000000000000007994 ) ;
#4511 = CARTESIAN_POINT ( 'NONE',  ( 1.500000000000001332, 7.960204194457796463E-16, -6.500000000000000888 ) ) ;
#4512 = DIRECTION ( 'NONE',  ( 0.000000000000000000, -1.000000000000000000, 0.000000000000000000 ) ) ;
#4513 = DIRECTION ( 'NONE',  ( -1.000000000000000000, -1.224606353822377258E-16, -0.000000000000000000 ) ) ;
#4514 = ORIENTED_EDGE ( 'NONE', *, *, #22502, .T. ) ;
#4515 = CARTESIAN_POINT ( 'NONE',  ( 33.99999999999998579, 5.999999999999985789, 11.00000000000000000 ) ) ;
#4516 = AXIS2_PLACEMENT_3D ( 'NONE', #12438, #20025, #14392 ) ;
#4517 = AXIS2_PLACEMENT_3D ( 'NONE', #3037, #19630, #6929 ) ;
#4518 = CARTESIAN_POINT ( 'NONE',  ( 47.34180362313352930, -5.000000000000016875, 9.500000000000000000 ) ) ;
#4519 = DIRECTION ( 'NONE',  ( 0.000000000000000000, -1.000000000000000000, 0.000000000000000000 ) ) ;
#4520 = EDGE_CURVE ( 'NONE', #21802, #7385, #15921, .T. ) ;
#4521 = DIRECTION ( 'NONE',  ( 0.000000000000000000, 0.000000000000000000, 1.000000000000000000 ) ) ;
#4522 = DIRECTION ( 'NONE',  ( -0.000000000000000000, -0.000000000000000000, -1.000000000000000000 ) ) ;
#4523 = CARTESIAN_POINT ( 'NONE',  ( -15.07341617659254496, 4.495283618570410589, 8.379779594489216166 ) ) ;
#4524 = CARTESIAN_POINT ( 'NONE',  ( -28.27483331787890819, -41.23752903419608629, 27.00000000000000000 ) ) ;
#4525 = EDGE_CURVE ( 'NONE', #13748, #22940, #8095, .T. ) ;
#4526 = ORIENTED_EDGE ( 'NONE', *, *, #17397, .F. ) ;
#4527 = CARTESIAN_POINT ( 'NONE',  ( -1.374911245008260563, 8.680847955710920161, -3.184419859656034024 ) ) ;
#4528 = CIRCLE ( 'NONE', #22041, 0.2999999999999999334 ) ;
#4529 = VERTEX_POINT ( 'NONE', #23495 ) ;
#4530 = CARTESIAN_POINT ( 'NONE',  ( -9.500000000000000000, -6.482511860946779655E-13, 11.05958914175814556 ) ) ;
#4531 = CARTESIAN_POINT ( 'NONE',  ( 2.024999999999999911, -45.00000000000000000, -27.00000000000000000 ) ) ;
#4532 = AXIS2_PLACEMENT_3D ( 'NONE', #3477, #12620, #20085 ) ;
#4533 = ORIENTED_EDGE ( 'NONE', *, *, #19701, .T. ) ;
#4534 = CARTESIAN_POINT ( 'NONE',  ( -2.682529543899159208, -8.255977015246598327, -12.03316557810918930 ) ) ;
#4535 = CARTESIAN_POINT ( 'NONE',  ( -9.000000000000000000, 0.000000000000000000, 15.50000000000000000 ) ) ;
#4536 = DIRECTION ( 'NONE',  ( -1.000000000000000000, -1.224606353822377258E-16, -0.000000000000000000 ) ) ;
#4537 = DIRECTION ( 'NONE',  ( 0.000000000000000000, 0.000000000000000000, -1.000000000000000000 ) ) ;
#4538 = CARTESIAN_POINT ( 'NONE',  ( 23.00000000000000000, 14.21257171757157245, 0.08908218613057176938 ) ) ;
#4539 = FACE_OUTER_BOUND ( 'NONE', #12573, .T. ) ;
#4540 = VECTOR ( 'NONE', #3036, 1000.000000000000227 ) ;
#4541 = DIRECTION ( 'NONE',  ( 0.000000000000000000, -1.000000000000000000, 0.000000000000000000 ) ) ;
#4542 = ORIENTED_EDGE ( 'NONE', *, *, #22522, .F. ) ;
#4543 = VECTOR ( 'NONE', #3395, 1000.000000000000000 ) ;
#4544 = VERTEX_POINT ( 'NONE', #13604 ) ;
#4545 = CARTESIAN_POINT ( 'NONE',  ( 60.03431729618309021, 5.000000000000015099, 0.000000000000000000 ) ) ;
#4546 = CARTESIAN_POINT ( 'NONE',  ( -41.00000000000000000, 6.000000000000000888, 12.00000000000000000 ) ) ;
#4547 = DIRECTION ( 'NONE',  ( -1.000000000000000000, 0.000000000000000000, 0.000000000000000000 ) ) ;
#4548 = VECTOR ( 'NONE', #12950, 1000.000000000000000 ) ;
#4549 = DIRECTION ( 'NONE',  ( -0.000000000000000000, -0.000000000000000000, -1.000000000000000000 ) ) ;
#4550 = EDGE_CURVE ( 'NONE', #5717, #18213, #13388, .T. ) ;
#4551 = ORIENTED_EDGE ( 'NONE', *, *, #10744, .F. ) ;
#4552 = EDGE_CURVE ( 'NONE', #10649, #12205, #21186, .T. ) ;
#4553 = DIRECTION ( 'NONE',  ( 1.000000000000000000, 0.000000000000000000, 0.000000000000000000 ) ) ;
#4554 = CARTESIAN_POINT ( 'NONE',  ( 61.48886275072855057, -5.000000000000000000, 6.123233995736775157E-16 ) ) ;
#4555 = ORIENTED_EDGE ( 'NONE', *, *, #8377, .F. ) ;
#4556 = CARTESIAN_POINT ( 'NONE',  ( -9.499999999999790390, -3.086737114213257804, -8.306742014460233747 ) ) ;
#4557 = EDGE_LOOP ( 'NONE', ( #19858, #9592, #10653, #9340 ) ) ;
#4558 = CARTESIAN_POINT ( 'NONE',  ( 23.00000000000000000, 12.00453763395396756, -1.558955687733494244 ) ) ;
#4559 = CARTESIAN_POINT ( 'NONE',  ( -8.680847955710813579, -2.820578480814257549, 11.73316557810918859 ) ) ;
#4560 = AXIS2_PLACEMENT_3D ( 'NONE', #4600, #17394, #11752 ) ;
#4561 = DIRECTION ( 'NONE',  ( 0.000000000000000000, 0.000000000000000000, 1.000000000000000000 ) ) ;
#4562 = PRODUCT_DEFINITION_FORMATION_WITH_SPECIFIED_SOURCE ( 'ANY', '', #19570, .NOT_KNOWN. ) ;
#4563 = DIRECTION ( 'NONE',  ( -0.000000000000000000, -0.000000000000000000, -1.000000000000000000 ) ) ;
#4564 = DIRECTION ( 'NONE',  ( 1.000000000000000000, 0.000000000000000000, 0.000000000000000000 ) ) ;
#4565 = AXIS2_PLACEMENT_3D ( 'NONE', #6953, #5113, #14376 ) ;
#4566 = EDGE_LOOP ( 'NONE', ( #4760, #17620, #21464, #12169 ) ) ;
#4567 = CARTESIAN_POINT ( 'NONE',  ( 1.500000000000001332, 0.000000000000000000, 0.000000000000000000 ) ) ;
#4568 = EDGE_CURVE ( 'NONE', #8063, #22874, #10771, .T. ) ;
#4569 = LINE ( 'NONE', #21392, #23469 ) ;
#4570 = ORIENTED_EDGE ( 'NONE', *, *, #20979, .T. ) ;
#4571 = PLANE ( 'NONE',  #550 ) ;
#4572 = EDGE_LOOP ( 'NONE', ( #5341, #20187, #19424, #21220 ) ) ;
#4573 = CARTESIAN_POINT ( 'NONE',  ( -2.808756108234559346, -9.079354608113304081, -3.500655287669418136 ) ) ;
#4574 = EDGE_CURVE ( 'NONE', #3226, #12189, #18079, .T. ) ;
#4575 = EDGE_CURVE ( 'NONE', #20997, #19575, #10270, .T. ) ;
#4576 = ORIENTED_EDGE ( 'NONE', *, *, #17794, .T. ) ;
#4577 = ADVANCED_FACE ( 'NONE', ( #11204, #3222 ), #18678, .F. ) ;
#4578 = CARTESIAN_POINT ( 'NONE',  ( -9.500000000000000000, 0.000000000000000000, 12.50000000000000000 ) ) ;
#4579 = EDGE_CURVE ( 'NONE', #17534, #3076, #12220, .T. ) ;
#4580 = DIRECTION ( 'NONE',  ( -1.000000000000000000, -1.224606353822377258E-16, -0.000000000000000000 ) ) ;
#4581 = DIRECTION ( 'NONE',  ( -1.000000000000000000, -0.000000000000000000, -0.000000000000000000 ) ) ;
#4582 =( BOUNDED_CURVE ( )  B_SPLINE_CURVE ( 3, ( #22808, #8132, #17169, #15095 ),
 .UNSPECIFIED., .F., .T. ) 
 B_SPLINE_CURVE_WITH_KNOTS ( ( 4, 4 ),
 ( 3.141592653589793116, 4.712388980384691450 ),
 .UNSPECIFIED. ) 
 CURVE ( )  GEOMETRIC_REPRESENTATION_ITEM ( )  RATIONAL_B_SPLINE_CURVE ( ( 1.000000000000000000, 0.8047378541243646044, 0.8047378541243646044, 1.000000000000000000 ) ) 
 REPRESENTATION_ITEM ( '' )  );
#4583 = PRODUCT_DEFINITION_CONTEXT ( 'detailed design', #6978, 'design' ) ;
#4584 = DIRECTION ( 'NONE',  ( -1.000000000000000000, 0.000000000000000000, 0.000000000000000000 ) ) ;
#4585 = ORIENTED_EDGE ( 'NONE', *, *, #9149, .T. ) ;
#4586 = CARTESIAN_POINT ( 'NONE',  ( 27.99999999999998934, -51.00000000000000711, 0.000000000000000000 ) ) ;
#4587 = DIRECTION ( 'NONE',  ( -0.000000000000000000, -0.000000000000000000, -1.000000000000000000 ) ) ;
#4588 = DIRECTION ( 'NONE',  ( -1.000000000000000000, -0.000000000000000000, -0.000000000000000000 ) ) ;
#4589 = EDGE_LOOP ( 'NONE', ( #8654, #14665, #12030, #2475 ) ) ;
#4590 = ORIENTED_EDGE ( 'NONE', *, *, #10272, .F. ) ;
#4591 = CARTESIAN_POINT ( 'NONE',  ( 7.685661446561619314, 5.583959896779020049, 10.25958914175814485 ) ) ;
#4592 = ORIENTED_EDGE ( 'NONE', *, *, #21779, .F. ) ;
#4593 = ORIENTED_EDGE ( 'NONE', *, *, #11991, .T. ) ;
#4594 = DIRECTION ( 'NONE',  ( -1.000000000000000000, -1.224606353822377258E-16, -0.000000000000000000 ) ) ;
#4595 = CARTESIAN_POINT ( 'NONE',  ( -8.680847955711200825, 2.820578480813073607, -5.533165578109187521 ) ) ;
#4596 = EDGE_CURVE ( 'NONE', #12531, #2253, #21889, .T. ) ;
#4597 = CARTESIAN_POINT ( 'NONE',  ( 0.000000000000000000, 6.242160243097294448, -9.879763041175060323 ) ) ;
#4598 = ORIENTED_EDGE ( 'NONE', *, *, #21097, .T. ) ;
#4599 = CARTESIAN_POINT ( 'NONE',  ( -17.49232137458054837, -9.205685982891289143, -2.395442301836272492 ) ) ;
#4600 = CARTESIAN_POINT ( 'NONE',  ( 58.57977184163763695, 7.562528597612068045E-15, 0.000000000000000000 ) ) ;
#4601 = CARTESIAN_POINT ( 'NONE',  ( 23.00000000000000000, 5.985147671565707483, 12.89120389306417103 ) ) ;
#4602 = DIRECTION ( 'NONE',  ( 1.000000000000000000, 0.000000000000000000, 0.000000000000000000 ) ) ;
#4603 = ORIENTED_EDGE ( 'NONE', *, *, #2740, .T. ) ;
#4604 = DIRECTION ( 'NONE',  ( 0.000000000000000000, 0.000000000000000000, 1.000000000000000000 ) ) ;
#4605 = LINE ( 'NONE', #23276, #12956 ) ;
#4606 = VERTEX_POINT ( 'NONE', #21665 ) ;
#4607 = CARTESIAN_POINT ( 'NONE',  ( 27.89784171216406961, 41.49349862090490859, -3.000000000000000000 ) ) ;
#4608 = ADVANCED_FACE ( 'NONE', ( #4962 ), #22477, .F. ) ;
#4609 = DIRECTION ( 'NONE',  ( -0.000000000000000000, -0.000000000000000000, -1.000000000000000000 ) ) ;
#4610 = CARTESIAN_POINT ( 'NONE',  ( 17.15242344757783499, -8.297343789534773251, -4.632629386303490193 ) ) ;
#4611 = CARTESIAN_POINT ( 'NONE',  ( 81.85249911436491743, 7.562528597612068045E-15, 0.000000000000000000 ) ) ;
#4612 = CARTESIAN_POINT ( 'NONE',  ( 5.365059087799947335, -7.384370330706356178, -8.333165578109188232 ) ) ;
#4613 = DIRECTION ( 'NONE',  ( 0.000000000000000000, 0.000000000000000000, 1.000000000000000000 ) ) ;
#4614 = ORIENTED_EDGE ( 'NONE', *, *, #17666, .F. ) ;
#4615 = ORIENTED_EDGE ( 'NONE', *, *, #7071, .F. ) ;
#4616 = CARTESIAN_POINT ( 'NONE',  ( -8.680847955710813579, -2.820578480814258437, -11.73316557810918859 ) ) ;
#4617 = CARTESIAN_POINT ( 'NONE',  ( -6.233975306307046963E-13, 9.127583699786111282, 11.13316557810918894 ) ) ;
#4618 = EDGE_LOOP ( 'NONE', ( #14958, #23511, #14689, #11711 ) ) ;
#4619 = DIRECTION ( 'NONE',  ( 0.9999997925849501978, 0.0006440730211827849078, -1.228571205523678748E-15 ) ) ;
#4620 = FACE_BOUND ( 'NONE', #9342, .T. ) ;
#4621 = ORIENTED_EDGE ( 'NONE', *, *, #16613, .T. ) ;
#4622 = DIRECTION ( 'NONE',  ( -0.000000000000000000, -0.000000000000000000, 1.000000000000000000 ) ) ;
#4623 = DIRECTION ( 'NONE',  ( -1.000000000000000000, 0.000000000000000000, 0.000000000000000000 ) ) ;
#4624 = CIRCLE ( 'NONE', #5379, 13.72592346138681130 ) ;
#4625 = CARTESIAN_POINT ( 'NONE',  ( 1.333298728199530769, 8.902595189562054756, 101.6946980188053118 ) ) ;
#4626 = DIRECTION ( 'NONE',  ( 1.000000000000000000, 0.000000000000000000, 0.000000000000000000 ) ) ;
#4627 = LINE ( 'NONE', #17165, #20859 ) ;
#4628 = EDGE_CURVE ( 'NONE', #14991, #15397, #4853, .T. ) ;
#4629 = ORIENTED_EDGE ( 'NONE', *, *, #6491, .T. ) ;
#4630 = DIRECTION ( 'NONE',  ( -1.000000000000000000, 0.000000000000000000, 0.000000000000000000 ) ) ;
#4631 = FACE_BOUND ( 'NONE', #20657, .T. ) ;
#4632 = ORIENTED_EDGE ( 'NONE', *, *, #17690, .T. ) ;
#4633 = DIRECTION ( 'NONE',  ( -1.000000000000000000, -0.000000000000000000, -0.000000000000000000 ) ) ;
#4634 = CARTESIAN_POINT ( 'NONE',  ( 0.2999999999999999334, 0.000000000000000000, 0.000000000000000000 ) ) ;
#4635 = EDGE_CURVE ( 'NONE', #15398, #19205, #8318, .T. ) ;
#4636 = CARTESIAN_POINT ( 'NONE',  ( 70.21613547800127719, 7.562528597612068045E-15, 0.000000000000000000 ) ) ;
#4637 = CARTESIAN_POINT ( 'NONE',  ( 0.000000000000000000, -11.55437235128772500, -1.752358929577761515 ) ) ;
#4638 = DIRECTION ( 'NONE',  ( 1.000000000000000000, 0.000000000000000000, 0.000000000000000000 ) ) ;
#4639 = ORIENTED_EDGE ( 'NONE', *, *, #7350, .F. ) ;
#4640 = CARTESIAN_POINT ( 'NONE',  ( -6.822232771736903637E-13, 9.988891130263535700, -11.70674201446023410 ) ) ;
#4641 = VECTOR ( 'NONE', #19698, 1000.000000000000000 ) ;
#4642 = VERTEX_POINT ( 'NONE', #14428 ) ;
#4643 = ORIENTED_EDGE ( 'NONE', *, *, #14603, .T. ) ;
#4644 = CARTESIAN_POINT ( 'NONE',  ( -9.500000000000000000, -6.482511860946779655E-13, 7.059589141758143782 ) ) ;
#4645 = CARTESIAN_POINT ( 'NONE',  ( 9.324366623732823450E-16, 6.000000000000000000, 80.99999999999998579 ) ) ;
#4646 = VERTEX_POINT ( 'NONE', #5177 ) ;
#4647 = SHAPE_REPRESENTATION_RELATIONSHIP ( 'NONE' , 'NONE' ,  #9527, #18921 ) ;
#4648 = DIRECTION ( 'NONE',  ( -0.8757121056631640421, -0.4828336235133042775, 0.000000000000000000 ) ) ;
#4649 = FACE_OUTER_BOUND ( 'NONE', #22896, .T. ) ;
#4650 = LINE ( 'NONE', #23680, #18554 ) ;
#4651 = DIRECTION ( 'NONE',  ( 1.000000000000000000, 0.000000000000000000, 0.000000000000000000 ) ) ;
#4652 = EDGE_CURVE ( 'NONE', #23565, #14989, #11417, .T. ) ;
#4653 = CARTESIAN_POINT ( 'NONE',  ( 14.51962751333974211, -3.765689428759034563, -8.721787840009190163 ) ) ;
#4654 = CARTESIAN_POINT ( 'NONE',  ( 41.99999999999999289, 25.93535998569253920, -27.00000000000000000 ) ) ;
#4655 = EDGE_CURVE ( 'NONE', #10789, #22991, #23, .T. ) ;
#4656 = VERTEX_POINT ( 'NONE', #20523 ) ;
#4657 = LINE ( 'NONE', #19531, #3185 ) ;
#4658 = EDGE_LOOP ( 'NONE', ( #12108, #18010, #13287, #23444 ) ) ;
#4659 = CARTESIAN_POINT ( 'NONE',  ( 86.51113724927145654, 7.420530141404717394E-15, 0.000000000000000000 ) ) ;
#4660 = DIRECTION ( 'NONE',  ( -1.000000000000000000, -0.000000000000000000, -0.000000000000000000 ) ) ;
#4661 = CARTESIAN_POINT ( 'NONE',  ( -5.622572944242077574E-13, 8.680847955711007202, 3.133165578109187610 ) ) ;
#4662 = DIRECTION ( 'NONE',  ( -0.000000000000000000, -0.000000000000000000, 1.000000000000000000 ) ) ;
#4663 = FACE_OUTER_BOUND ( 'NONE', #23790, .T. ) ;
#4664 = ORIENTED_EDGE ( 'NONE', *, *, #18556, .T. ) ;
#4665 = CARTESIAN_POINT ( 'NONE',  ( -1.499999999999998668, 2.143131898507867311E-16, 0.000000000000000000 ) ) ;
#4666 = EDGE_LOOP ( 'NONE', ( #16735, #6778, #2061, #17543 ) ) ;
#4667 = CARTESIAN_POINT ( 'NONE',  ( -7.685661446561619314, -5.583959896779019161, -8.406742014460233392 ) ) ;
#4668 = ORIENTED_EDGE ( 'NONE', *, *, #8058, .F. ) ;
#4669 = CARTESIAN_POINT ( 'NONE',  ( -41.50000000000000000, -28.80990663662250739, 0.000000000000000000 ) ) ;
#4670 = CARTESIAN_POINT ( 'NONE',  ( -42.00000000000000000, -6.000000000000000888, 10.49999999999999822 ) ) ;
#4671 = DIRECTION ( 'NONE',  ( -0.000000000000000000, -0.000000000000000000, 1.000000000000000000 ) ) ;
#4672 = FACE_OUTER_BOUND ( 'NONE', #11882, .T. ) ;
#4673 = AXIS2_PLACEMENT_3D ( 'NONE', #8100, #805, #19363 ) ;
#4674 = LINE ( 'NONE', #12079, #18912 ) ;
#4675 = EDGE_CURVE ( 'NONE', #18344, #10068, #3797, .T. ) ;
#4676 = CONTEXT_DEPENDENT_SHAPE_REPRESENTATION ( #21347, #5556 ) ;
#4677 = EDGE_CURVE ( 'NONE', #21210, #4271, #10645, .T. ) ;
#4678 = DIRECTION ( 'NONE',  ( -1.000000000000000000, -1.224606353822377258E-16, -0.000000000000000000 ) ) ;
#4679 = ADVANCED_FACE ( 'NONE', ( #2711 ), #22776, .F. ) ;
#4680 = AXIS2_PLACEMENT_3D ( 'NONE', #847, #980, #15589 ) ;
#4681 = CARTESIAN_POINT ( 'NONE',  ( -7.685661446561619314, -5.583959896779019161, -12.40674201446023339 ) ) ;
#4682 = ORIENTED_EDGE ( 'NONE', *, *, #23890, .F. ) ;
#4683 = DIRECTION ( 'NONE',  ( -1.000000000000000000, -1.224606353822377258E-16, -0.000000000000000000 ) ) ;
#4684 = CIRCLE ( 'NONE', #15953, 2.024999999999999911 ) ;
#4685 = DIRECTION ( 'NONE',  ( 0.000000000000000000, 1.000000000000000000, 0.000000000000000000 ) ) ;
#4686 = DIRECTION ( 'NONE',  ( -0.000000000000000000, -0.000000000000000000, -1.000000000000000000 ) ) ;
#4687 = ORIENTED_EDGE ( 'NONE', *, *, #20366, .F. ) ;
#4688 = CARTESIAN_POINT ( 'NONE',  ( 78.36363636363637397, 7.491529369508391930E-15, 0.000000000000000000 ) ) ;
#4689 = DIRECTION ( 'NONE',  ( 1.000000000000000000, 0.000000000000000000, 0.000000000000000000 ) ) ;
#4690 = DIRECTION ( 'NONE',  ( 0.000000000000000000, 0.000000000000000000, -1.000000000000000000 ) ) ;
#4691 = DIRECTION ( 'NONE',  ( -1.000000000000000000, -0.000000000000000000, -0.000000000000000000 ) ) ;
#4692 = DIRECTION ( 'NONE',  ( -1.000000000000000000, -0.000000000000000000, -0.000000000000000000 ) ) ;
#4693 = EDGE_LOOP ( 'NONE', ( #13020, #19682, #729, #400 ) ) ;
#4694 = DIRECTION ( 'NONE',  ( -0.000000000000000000, 0.000000000000000000, -1.000000000000000000 ) ) ;
#4695 = DIRECTION ( 'NONE',  ( -1.000000000000000000, 0.000000000000000000, 0.000000000000000000 ) ) ;
#4696 = CARTESIAN_POINT ( 'NONE',  ( -9.500000000000000000, -6.482511860946779655E-13, -5.059589141758143782 ) ) ;
#4697 = ORIENTED_EDGE ( 'NONE', *, *, #8220, .F. ) ;
#4698 = PRODUCT_RELATED_PRODUCT_CATEGORY ( 'part', '', ( #3416 ) ) ;
#4699 = CARTESIAN_POINT ( 'NONE',  ( 9.500000000000209610, -3.086737114211962396, 7.959589141758143249 ) ) ;
#4700 = EDGE_CURVE ( 'NONE', #8062, #21512, #12076, .T. ) ;
#4701 = AXIS2_PLACEMENT_3D ( 'NONE', #8162, #15605, #5427 ) ;
#4702 = VERTEX_POINT ( 'NONE', #23349 ) ;
#4703 = VERTEX_POINT ( 'NONE', #4798 ) ;
#4704 = ORIENTED_EDGE ( 'NONE', *, *, #21763, .T. ) ;
#4705 = VERTEX_POINT ( 'NONE', #10009 ) ;
#4706 = ADVANCED_FACE ( 'NONE', ( #17466 ), #6808, .F. ) ;
#4707 = DIRECTION ( 'NONE',  ( -0.000000000000000000, -0.000000000000000000, 1.000000000000000000 ) ) ;
#4708 = EDGE_CURVE ( 'NONE', #11663, #760, #21995, .T. ) ;
#4709 = DIRECTION ( 'NONE',  ( 1.000000000000000000, 0.000000000000000000, 0.000000000000000000 ) ) ;
#4710 = CARTESIAN_POINT ( 'NONE',  ( 34.10000000000000142, 29.50000000000000355, 12.00000000000000000 ) ) ;
#4711 = VERTEX_POINT ( 'NONE', #21749 ) ;
#4712 = CARTESIAN_POINT ( 'NONE',  ( -17.59041996266973129, -9.500503876990130436, -0.4759723220310695391 ) ) ;
#4713 = DIRECTION ( 'NONE',  ( 0.000000000000000000, 0.000000000000000000, -1.000000000000000000 ) ) ;
#4714 = CARTESIAN_POINT ( 'NONE',  ( 40.00000000000000000, 0.000000000000000000, 12.00000000000000000 ) ) ;
#4715 = LINE ( 'NONE', #1175, #21803 ) ;
#4716 = ORIENTED_EDGE ( 'NONE', *, *, #19691, .F. ) ;
#4717 = CARTESIAN_POINT ( 'NONE',  ( 0.000000000000000000, -0.09016380984455869829, -11.68615217844040721 ) ) ;
#4718 =( BOUNDED_CURVE ( )  B_SPLINE_CURVE ( 2, ( #4696, #16146, #912, #2622, #3099, #15645, #21411, #790, #5057, #21772, #4950 ),
 .UNSPECIFIED., .F., .T. ) 
 B_SPLINE_CURVE_WITH_KNOTS ( ( 3, 2, 2, 2, 2, 3 ),
 ( 0.7000000000000000666, 0.7200000000000000844, 0.7400000000000001021, 0.7600000000000000089, 0.7800000000000000266, 0.8000000000000000444 ),
 .UNSPECIFIED. ) 
 CURVE ( )  GEOMETRIC_REPRESENTATION_ITEM ( )  RATIONAL_B_SPLINE_CURVE ( ( 0.9999999999999997780, 0.9510565162951537532, 1.000000000000000000, 0.9510565162951535312, 1.000000000000000000, 0.9510565162951535312, 1.000000000000000000, 0.9510565162951535312, 1.000000000000000000, 0.9510565162951535312, 1.000000000000000000 ) ) 
 REPRESENTATION_ITEM ( '' )  );
#4719 = DIRECTION ( 'NONE',  ( -0.000000000000000000, -1.000000000000000000, -0.000000000000000000 ) ) ;
#4720 = DIRECTION ( 'NONE',  ( -1.000000000000000000, 0.000000000000000000, 0.000000000000000000 ) ) ;
#4721 = VECTOR ( 'NONE', #20899, 1000.000000000000000 ) ;
#4722 = DIRECTION ( 'NONE',  ( -1.000000000000000000, -0.000000000000000000, -0.000000000000000000 ) ) ;
#4723 = CARTESIAN_POINT ( 'NONE',  ( -20.99999999999999645, -29.49999999999999645, 12.00000000000000000 ) ) ;
#4724 = DIRECTION ( 'NONE',  ( -1.000000000000000000, 0.000000000000000000, 0.000000000000000000 ) ) ;
#4725 = CARTESIAN_POINT ( 'NONE',  ( 14.67173559926287929, 3.179195828807838353, 8.975010320294691368 ) ) ;
#4726 = CARTESIAN_POINT ( 'NONE',  ( -6.233975306307045953E-13, 9.127583699786111282, -9.133165578109188942 ) ) ;
#4727 = LINE ( 'NONE', #14223, #16392 ) ;
#4728 = EDGE_LOOP ( 'NONE', ( #4592, #20960, #14578, #23218, #16275 ) ) ;
#4729 = ADVANCED_FACE ( 'NONE', ( #12694, #22121 ), #20037, .F. ) ;
#4730 = ORIENTED_EDGE ( 'NONE', *, *, #5566, .T. ) ;
#4731 = CARTESIAN_POINT ( 'NONE',  ( 8.680847955711007202, 5.912916378492122225E-13, 12.63316557810918894 ) ) ;
#4732 = ORIENTED_EDGE ( 'NONE', *, *, #2343, .T. ) ;
#4733 = DIRECTION ( 'NONE',  ( -0.9999999999999998890, 0.000000000000000000, 0.000000000000000000 ) ) ;
#4734 = CARTESIAN_POINT ( 'NONE',  ( -7.561939491010498671, 5.750397476200742375, -11.99999999999999822 ) ) ;
#4735 = CIRCLE ( 'NONE', #18354, 10.99999999999999645 ) ;
#4736 = ORIENTED_EDGE ( 'NONE', *, *, #6012, .T. ) ;
#4737 = VERTEX_POINT ( 'NONE', #21627 ) ;
#4738 = EDGE_CURVE ( 'NONE', #20131, #23091, #12449, .T. ) ;
#4739 = DIRECTION ( 'NONE',  ( 0.5735764363510424957, 0.8191520442889943521, 0.000000000000000000 ) ) ;
#4740 = DIRECTION ( 'NONE',  ( 1.000000000000000000, 0.000000000000000000, 0.000000000000000000 ) ) ;
#4741 = UNCERTAINTY_MEASURE_WITH_UNIT (LENGTH_MEASURE( 1.000000000000000082E-05 ), #13544, 'distance_accuracy_value', 'NONE');
#4742 = EDGE_CURVE ( 'NONE', #13221, #22169, #171, .T. ) ;
#4743 = AXIS2_PLACEMENT_3D ( 'NONE', #13130, #18386, #7284 ) ;
#4744 = DIRECTION ( 'NONE',  ( -1.000000000000000000, -0.000000000000000000, -0.000000000000000000 ) ) ;
#4745 = DIRECTION ( 'NONE',  ( 1.000000000000000000, -4.613626265895764052E-16, 0.000000000000000000 ) ) ;
#4746 = DIRECTION ( 'NONE',  ( -0.000000000000000000, -0.000000000000000000, -1.000000000000000000 ) ) ;
#4747 = ORIENTED_EDGE ( 'NONE', *, *, #4802, .T. ) ;
#4748 = ORIENTED_EDGE ( 'NONE', *, *, #15937, .T. ) ;
#4749 = LINE ( 'NONE', #23659, #18427 ) ;
#4750 = DIRECTION ( 'NONE',  ( 0.000000000000000000, 0.9096319953545193293, -0.4154150130018841591 ) ) ;
#4751 = ORIENTED_EDGE ( 'NONE', *, *, #18066, .F. ) ;
#4752 = CYLINDRICAL_SURFACE ( 'NONE', #6298, 1.000000000000000888 ) ;
#4753 = ORIENTED_EDGE ( 'NONE', *, *, #2367, .F. ) ;
#4754 = LINE ( 'NONE', #7037, #4794 ) ;
#4755 = CYLINDRICAL_SURFACE ( 'NONE', #18824, 23.85000000000000497 ) ;
#4756 = FACE_OUTER_BOUND ( 'NONE', #14452, .T. ) ;
#4757 = ORIENTED_EDGE ( 'NONE', *, *, #19144, .T. ) ;
#4758 = CIRCLE ( 'NONE', #23880, 4.172000000000008590 ) ;
#4759 = CIRCLE ( 'NONE', #16412, 6.050000000006050982 ) ;
#4760 = ORIENTED_EDGE ( 'NONE', *, *, #22229, .F. ) ;
#4761 = ORIENTED_EDGE ( 'NONE', *, *, #13853, .F. ) ;
#4762 = CARTESIAN_POINT ( 'NONE',  ( 2.935661446562616295, -9.035036904803758873, 12.80674201446023375 ) ) ;
#4763 = CARTESIAN_POINT ( 'NONE',  ( 5.871322893124553133, -8.081182679343980269, 12.90674201446023517 ) ) ;
#4764 = ORIENTED_EDGE ( 'NONE', *, *, #16506, .F. ) ;
#4765 = CARTESIAN_POINT ( 'NONE',  ( -36.00000000000001421, 50.99999999999999289, 0.5000000000000000000 ) ) ;
#4766 = CARTESIAN_POINT ( 'NONE',  ( 7.999999999999992895, 1.040949779275249943E-15, 105.0000000000000000 ) ) ;
#4767 = DIRECTION ( 'NONE',  ( -0.5735764363510517105, -0.8191520442889879128, 0.000000000000000000 ) ) ;
#4768 = EDGE_CURVE ( 'NONE', #13833, #5846, #15995, .T. ) ;
#4769 = AXIS2_PLACEMENT_3D ( 'NONE', #15579, #15956, #23044 ) ;
#4770 = CARTESIAN_POINT ( 'NONE',  ( 33.99999999999998579, -1.387778780781445676E-14, 9.500000000000000000 ) ) ;
#4771 = AXIS2_PLACEMENT_3D ( 'NONE', #12297, #1564, #16421 ) ;
#4772 = CARTESIAN_POINT ( 'NONE',  ( -21.13207267780287069, 38.32709852940855910, 12.00000000000000000 ) ) ;
#4773 = CARTESIAN_POINT ( 'NONE',  ( 0.000000000000000000, 0.000000000000000000, 12.50000000000000000 ) ) ;
#4774 = PRODUCT_DEFINITION_SHAPE ( 'NONE', 'NONE',  #24108 ) ;
#4775 = CIRCLE ( 'NONE', #11350, 4.172000000000008590 ) ;
#4776 = VERTEX_POINT ( 'NONE', #20163 ) ;
#4777 = CARTESIAN_POINT ( 'NONE',  ( 77.48886275072855767, 7.562528597612068045E-15, 0.000000000000000000 ) ) ;
#4778 = VERTEX_POINT ( 'NONE', #3078 ) ;
#4779 = DIRECTION ( 'NONE',  ( -1.000000000000000000, -1.224606353822377258E-16, -0.000000000000000000 ) ) ;
#4780 = DIRECTION ( 'NONE',  ( -0.000000000000000000, -0.000000000000000000, -1.000000000000000000 ) ) ;
#4781 = CYLINDRICAL_SURFACE ( 'NONE', #21138, 5.100000000000000533 ) ;
#4782 = CARTESIAN_POINT ( 'NONE',  ( 82.14750088563508257, 5.000000000000025757, 6.123233995736788962E-16 ) ) ;
#4783 = DIRECTION ( 'NONE',  ( 0.000000000000000000, 0.000000000000000000, -1.000000000000000000 ) ) ;
#4784 = ORIENTED_EDGE ( 'NONE', *, *, #15456, .F. ) ;
#4785 = EDGE_CURVE ( 'NONE', #16706, #6136, #12621, .T. ) ;
#4786 = CARTESIAN_POINT ( 'NONE',  ( -9.500000000000202505, 3.086737114211975275, 8.959589141758142361 ) ) ;
#4787 = ORIENTED_EDGE ( 'NONE', *, *, #247, .F. ) ;
#4788 = DIRECTION ( 'NONE',  ( 0.000000000000000000, -1.000000000000000000, 0.000000000000000000 ) ) ;
#4789 = VECTOR ( 'NONE', #5458, 1000.000000000000227 ) ;
#4790 = ORIENTED_EDGE ( 'NONE', *, *, #6630, .T. ) ;
#4791 = EDGE_CURVE ( 'NONE', #8445, #2607, #14519, .T. ) ;
#4792 = LINE ( 'NONE', #10607, #15263 ) ;
#4793 = VECTOR ( 'NONE', #14520, 1000.000000000000000 ) ;
#4794 = VECTOR ( 'NONE', #14467, 1000.000000000000000 ) ;
#4795 = CIRCLE ( 'NONE', #18413, 11.23082370883260062 ) ;
#4796 = DIRECTION ( 'NONE',  ( -1.000000000000000000, -1.224606353822377258E-16, -0.000000000000000000 ) ) ;
#4797 = VECTOR ( 'NONE', #8329, 1000.000000000000000 ) ;
#4798 = CARTESIAN_POINT ( 'NONE',  ( 0.000000000000000000, -14.96647757894464270, 6.750000000000000888 ) ) ;
#4799 = EDGE_CURVE ( 'NONE', #10396, #20942, #9874, .T. ) ;
#4800 = AXIS2_PLACEMENT_3D ( 'NONE', #12360, #20059, #22013 ) ;
#4801 = LINE ( 'NONE', #17468, #9200 ) ;
#4802 = EDGE_CURVE ( 'NONE', #17959, #7789, #2499, .T. ) ;
#4803 = CARTESIAN_POINT ( 'NONE',  ( -9.500000000000000000, -6.482511860946779655E-13, 5.059589141758143782 ) ) ;
#4804 = EDGE_LOOP ( 'NONE', ( #19717, #368, #1032, #6560 ) ) ;
#4805 = ITEM_DEFINED_TRANSFORMATION ( 'NONE', 'NONE', #4944,  #8005 ) ;
#4806 = VERTEX_POINT ( 'NONE', #18779 ) ;
#4807 = DIRECTION ( 'NONE',  ( -0.000000000000000000, -0.000000000000000000, 1.000000000000000000 ) ) ;
#4808 = EDGE_LOOP ( 'NONE', ( #9400, #10254 ) ) ;
#4809 = AXIS2_PLACEMENT_3D ( 'NONE', #21341, #8752, #19980 ) ;
#4810 = CARTESIAN_POINT ( 'NONE',  ( 0.000000000000000000, 1.803405503031483077E-15, -14.72592346043842326 ) ) ;
#4811 = AXIS2_PLACEMENT_3D ( 'NONE', #693, #8099, #4477 ) ;
#4812 = TOROIDAL_SURFACE ( 'NONE', #22730, 49.00000000000000000, 1.000000000000000000 ) ;
#4813 = VERTEX_POINT ( 'NONE', #9154 ) ;
#4814 = DIRECTION ( 'NONE',  ( -1.000000000000000000, -0.000000000000000000, -0.000000000000000000 ) ) ;
#4815 = CIRCLE ( 'NONE', #14518, 1.000000000000000888 ) ;
#4816 = CIRCLE ( 'NONE', #7122, 4.172000000000008590 ) ;
#4817 = EDGE_LOOP ( 'NONE', ( #8716, #22684, #218, #2995, #7852, #22603 ) ) ;
#4818 = DIRECTION ( 'NONE',  ( -0.000000000000000000, -0.000000000000000000, -1.000000000000000000 ) ) ;
#4819 = DIRECTION ( 'NONE',  ( 0.000000000000000000, -1.000000000000000000, 0.000000000000000000 ) ) ;
#4820 = AXIS2_PLACEMENT_3D ( 'NONE', #3851, #22633, #2007 ) ;
#4821 = DIRECTION ( 'NONE',  ( 0.000000000000000000, 0.000000000000000000, 1.000000000000000000 ) ) ;
#4822 = CARTESIAN_POINT ( 'NONE',  ( 0.000000000000000000, 0.000000000000000000, 12.50000000000000000 ) ) ;
#4823 = DIRECTION ( 'NONE',  ( -1.000000000000000000, 0.000000000000000000, 0.000000000000000000 ) ) ;
#4824 = ORIENTED_EDGE ( 'NONE', *, *, #9907, .F. ) ;
#4825 = APPLICATION_CONTEXT ( 'automotive_design' ) ;
#4826 = DIRECTION ( 'NONE',  ( -1.000000000000000000, -1.224606353822377258E-16, -0.000000000000000000 ) ) ;
#4827 = EDGE_CURVE ( 'NONE', #21873, #3596, #22686, .T. ) ;
#4828 = DIRECTION ( 'NONE',  ( -0.000000000000000000, -0.000000000000000000, -1.000000000000000000 ) ) ;
#4829 = EDGE_CURVE ( 'NONE', #12080, #2862, #9495, .T. ) ;
#4830 = CARTESIAN_POINT ( 'NONE',  ( 58.57977184163763695, 6.123233995736675563E-16, -5.000000000000007994 ) ) ;
#4831 = CARTESIAN_POINT ( 'NONE',  ( -2.935661446562617183, 9.035036904803758873, 8.659589141758143427 ) ) ;
#4832 = VECTOR ( 'NONE', #277, 1000.000000000000000 ) ;
#4833 = AXIS2_PLACEMENT_3D ( 'NONE', #8871, #4882, #16312 ) ;
#4834 = CONICAL_SURFACE ( 'NONE', #17272, 39.49999999999999289, 0.7853981633974621568 ) ;
#4835 = VECTOR ( 'NONE', #5581, 1000.000000000000000 ) ;
#4836 = CIRCLE ( 'NONE', #2478, 14.99999999999999822 ) ;
#4837 = VERTEX_POINT ( 'NONE', #18922 ) ;
#4838 = CYLINDRICAL_SURFACE ( 'NONE', #23268, 5.000000000000000888 ) ;
#4839 = TOROIDAL_SURFACE ( 'NONE', #6370, 5.999999999999999112, 1.000000000000000000 ) ;
#4840 = CARTESIAN_POINT ( 'NONE',  ( 66.72727272727273373, -4.172000000000000597, 0.000000000000000000 ) ) ;
#4841 = CARTESIAN_POINT ( 'NONE',  ( -0.9830802669677229932, 45.00000000000000000, 0.000000000000000000 ) ) ;
#4842 = CARTESIAN_POINT ( 'NONE',  ( -16.68233279685676607, -7.225448002938850145, 6.184784653374924446 ) ) ;
#4843 = CARTESIAN_POINT ( 'NONE',  ( -31.74999999999995737, 0.000000000000000000, 0.000000000000000000 ) ) ;
#4844 = VERTEX_POINT ( 'NONE', #10956 ) ;
#4845 = FACE_OUTER_BOUND ( 'NONE', #15467, .T. ) ;
#4846 = CARTESIAN_POINT ( 'NONE',  ( 9.500000000000209610, -3.086737114211962396, 7.959589141758143249 ) ) ;
#4847 = CARTESIAN_POINT ( 'NONE',  ( -9.500000000000211386, 3.086737114211961064, 6.106742014460234458 ) ) ;
#4848 = CARTESIAN_POINT ( 'NONE',  ( 41.99999999999997158, -25.22443390181681622, -1.500000000000000000 ) ) ;
#4849 = CARTESIAN_POINT ( 'NONE',  ( -1.999999999999997113, 45.00000000000000000, -2.974999999999996092 ) ) ;
#4850 = AXIS2_PLACEMENT_3D ( 'NONE', #8191, #23246, #2850 ) ;
#4851 = ADVANCED_FACE ( 'NONE', ( #16712 ), #9122, .T. ) ;
#4852 = LINE ( 'NONE', #17777, #18539 ) ;
#4853 = CIRCLE ( 'NONE', #11037, 4.057500000000000107 ) ;
#4854 = CARTESIAN_POINT ( 'NONE',  ( -29.00000000000000000, 29.49999999999999645, 0.000000000000000000 ) ) ;
#4855 = EDGE_CURVE ( 'NONE', #2378, #20352, #24048, .T. ) ;
#4856 = VECTOR ( 'NONE', #16499, 1000.000000000000000 ) ;
#4857 = FACE_OUTER_BOUND ( 'NONE', #3861, .T. ) ;
#4858 = EDGE_CURVE ( 'NONE', #6705, #2772, #19675, .T. ) ;
#4859 = DIRECTION ( 'NONE',  ( -0.7071067811865493491, 8.659560562354955045E-17, 0.7071067811865456854 ) ) ;
#4860 = EDGE_LOOP ( 'NONE', ( #4025, #12431, #8164, #982 ) ) ;
#4861 = AXIS2_PLACEMENT_3D ( 'NONE', #20119, #16314, #9110 ) ;
#4862 = CARTESIAN_POINT ( 'NONE',  ( -8.680847955711200825, 2.820578480813073607, -11.53316557810918574 ) ) ;
#4863 = VERTEX_POINT ( 'NONE', #7424 ) ;
#4864 = DIRECTION ( 'NONE',  ( -1.665334536937734811E-16, 1.110223024625156540E-16, 0.9999999999999997780 ) ) ;
#4865 = DIRECTION ( 'NONE',  ( -0.000000000000000000, -0.000000000000000000, -1.000000000000000000 ) ) ;
#4866 = ORIENTED_EDGE ( 'NONE', *, *, #6503, .F. ) ;
#4867 = CARTESIAN_POINT ( 'NONE',  ( 0.000000000000000000, 17.26667456984545268, -4.623588898214372911 ) ) ;
#4868 = CARTESIAN_POINT ( 'NONE',  ( 9.500000000000209610, -3.086737114211962396, -7.959589141758143249 ) ) ;
#4869 = CONICAL_SURFACE ( 'NONE', #5631, 4.172000000000008590, 0.9599310885968742602 ) ;
#4870 = AXIS2_PLACEMENT_3D ( 'NONE', #618, #2315, #4648 ) ;
#4871 = CARTESIAN_POINT ( 'NONE',  ( 2.901639506146888703, 8.519518907301963040, 99.78718033059439563 ) ) ;
#4872 = DIRECTION ( 'NONE',  ( -0.000000000000000000, 0.000000000000000000, 1.000000000000000000 ) ) ;
#4873 = CARTESIAN_POINT ( 'NONE',  ( -6.153822176767817416E-13, 9.500000000000000000, 3.499999999999999556 ) ) ;
#4874 = VECTOR ( 'NONE', #18326, 1000.000000000000000 ) ;
#4875 = CARTESIAN_POINT ( 'NONE',  ( 79.23840997654417606, 7.420530141404717394E-15, 0.000000000000000000 ) ) ;
#4876 = ADVANCED_FACE ( 'NONE', ( #5625 ), #13050, .T. ) ;
#4877 = AXIS2_PLACEMENT_3D ( 'NONE', #14940, #5451, #9222 ) ;
#4878 = CARTESIAN_POINT ( 'NONE',  ( 9.330908268522556170, -1.784418920662232289, 11.99999999999997691 ) ) ;
#4879 = CARTESIAN_POINT ( 'NONE',  ( -43.49999999999997868, -25.84341543330624091, 0.000000000000000000 ) ) ;
#4880 = EDGE_LOOP ( 'NONE', ( #12878, #6273 ) ) ;
#4881 = DIRECTION ( 'NONE',  ( 1.000000000000000000, 0.000000000000000000, 0.000000000000000000 ) ) ;
#4882 = DIRECTION ( 'NONE',  ( -0.000000000000000000, -0.000000000000000000, 1.000000000000000000 ) ) ;
#4883 = DIRECTION ( 'NONE',  ( 1.000000000000000000, 0.000000000000000000, 0.000000000000000000 ) ) ;
#4884 = EDGE_CURVE ( 'NONE', #2345, #8087, #5238, .T. ) ;
#4885 = VERTEX_POINT ( 'NONE', #20623 ) ;
#4886 = CARTESIAN_POINT ( 'NONE',  ( 7.022953521755574080, -5.102474405759714671, -4.433165578109187877 ) ) ;
#4887 = ADVANCED_FACE ( 'NONE', ( #19042 ), #6333, .F. ) ;
#4888 = CIRCLE ( 'NONE', #5651, 15.00000000000000000 ) ;
#4889 = ORIENTED_EDGE ( 'NONE', *, *, #17436, .F. ) ;
#4890 = AXIS2_PLACEMENT_3D ( 'NONE', #14284, #3178, #4788 ) ;
#4891 = ORIENTED_EDGE ( 'NONE', *, *, #2690, .F. ) ;
#4892 = CARTESIAN_POINT ( 'NONE',  ( 7.685661446562381371, -5.583959896777971110, 3.859589141758143604 ) ) ;
#4893 = CARTESIAN_POINT ( 'NONE',  ( -9.500000000000000000, -6.482511860946779655E-13, 4.206742014460233214 ) ) ;
#4894 = AXIS2_PLACEMENT_3D ( 'NONE', #3017, #15817, #21188 ) ;
#4895 = ORIENTED_EDGE ( 'NONE', *, *, #9250, .F. ) ;
#4896 = CIRCLE ( 'NONE', #215, 9.500000000000000000 ) ;
#4897 = DIRECTION ( 'NONE',  ( -1.000000000000000000, -0.000000000000000000, -0.000000000000000000 ) ) ;
#4898 = CARTESIAN_POINT ( 'NONE',  ( 28.27483331787887977, 41.23752903419610760, 0.000000000000000000 ) ) ;
#4899 = AXIS2_PLACEMENT_3D ( 'NONE', #18020, #1316, #19383 ) ;
#4900 = AXIS2_PLACEMENT_3D ( 'NONE', #349, #19021, #7763 ) ;
#4901 = CARTESIAN_POINT ( 'NONE',  ( -24.75000000000000000, -29.50000000000000000, 12.50000000000000000 ) ) ;
#4902 = CARTESIAN_POINT ( 'NONE',  ( -14.99999999999999822, 0.000000000000000000, -27.00000000000000000 ) ) ;
#4903 = CARTESIAN_POINT ( 'NONE',  ( -40.89823313241237912, -26.41789760203349502, -27.00000000000000000 ) ) ;
#4904 = DIRECTION ( 'NONE',  ( 1.000000000000000000, -0.000000000000000000, 0.000000000000000000 ) ) ;
#4905 = EDGE_CURVE ( 'NONE', #498, #6272, #9978, .T. ) ;
#4906 = EDGE_LOOP ( 'NONE', ( #12601, #23933, #1457, #12156 ) ) ;
#4907 = DIRECTION ( 'NONE',  ( -0.000000000000000000, -0.000000000000000000, -1.000000000000000000 ) ) ;
#4908 = CARTESIAN_POINT ( 'NONE',  ( 9.500000000000000000, 6.470877716354879437E-13, -10.05958914175814378 ) ) ;
#4909 = DIRECTION ( 'NONE',  ( -0.8757121056631633760, 0.4828336235133056653, 0.000000000000000000 ) ) ;
#4911 = CARTESIAN_POINT ( 'NONE',  ( -7.685661446561619314, -5.583959896779019161, 11.25958914175814307 ) ) ;
#4910 = CIRCLE ( 'NONE', #18533, 11.68650000001168721 ) ;
#4912 = FILL_AREA_STYLE_COLOUR ( '', #21789 ) ;
#4913 = EDGE_CURVE ( 'NONE', #5821, #7706, #18482, .T. ) ;
#4914 = CIRCLE ( 'NONE', #8403, 39.49999999999999289 ) ;
#4915 = CARTESIAN_POINT ( 'NONE',  ( 0.000000000000000000, 11.90821470209334798, -7.758837095328730449 ) ) ;
#4916 = ORIENTED_EDGE ( 'NONE', *, *, #11662, .F. ) ;
#4917 = EDGE_CURVE ( 'NONE', #3022, #6856, #7938, .T. ) ;
#4918 = CARTESIAN_POINT ( 'NONE',  ( 74.87477361290781630, -4.999999999999989342, 0.000000000000000000 ) ) ;
#4919 = CIRCLE ( 'NONE', #2157, 15.00000000000000000 ) ;
#4920 = VERTEX_POINT ( 'NONE', #6102 ) ;
#4921 = CARTESIAN_POINT ( 'NONE',  ( 2.935661446561383503, 9.035036904804158553, -6.459589141758144137 ) ) ;
#4922 = VERTEX_POINT ( 'NONE', #12049 ) ;
#4923 = CARTESIAN_POINT ( 'NONE',  ( -2.682529543900285862, 8.255977015246234174, 3.233165578109188587 ) ) ;
#4924 = VERTEX_POINT ( 'NONE', #8147 ) ;
#4925 = DIRECTION ( 'NONE',  ( -1.000000000000000000, -1.224606353822377258E-16, -0.000000000000000000 ) ) ;
#4926 = CYLINDRICAL_SURFACE ( 'NONE', #19191, 9.000000000000000000 ) ;
#4927 = DIRECTION ( 'NONE',  ( 0.000000000000000000, -1.000000000000000000, 0.000000000000000000 ) ) ;
#4928 = CIRCLE ( 'NONE', #20491, 9.500000000000000000 ) ;
#4929 = CARTESIAN_POINT ( 'NONE',  ( 0.000000000000000000, -15.23000000000000220, 27.00000000000000000 ) ) ;
#4930 = AXIS2_PLACEMENT_3D ( 'NONE', #19933, #18591, #1866 ) ;
#4931 = CARTESIAN_POINT ( 'NONE',  ( 9.500000000000209610, -3.086737114211962396, -7.106742014460232681 ) ) ;
#4932 = ORIENTED_EDGE ( 'NONE', *, *, #21763, .F. ) ;
#4933 = ORIENTED_EDGE ( 'NONE', *, *, #7581, .F. ) ;
#4934 = CARTESIAN_POINT ( 'NONE',  ( -8.539523583899518044, -3.764097148612461474, -12.19964644692132438 ) ) ;
#4935 = EDGE_CURVE ( 'NONE', #7050, #15853, #18866, .T. ) ;
#4936 = CARTESIAN_POINT ( 'NONE',  ( 73.12522638709218370, -1.078520768856852078E-29, 5.000000000000007994 ) ) ;
#4937 = ADVANCED_FACE ( 'NONE', ( #20987 ), #22946, .T. ) ;
#4938 = VERTEX_POINT ( 'NONE', #9858 ) ;
#4939 = CONICAL_SURFACE ( 'NONE', #2181, 2.024999999999999911, 0.7853981633974743692 ) ;
#4940 = FACE_OUTER_BOUND ( 'NONE', #323, .T. ) ;
#4941 = EDGE_CURVE ( 'NONE', #14876, #15606, #6217, .T. ) ;
#4942 = DIRECTION ( 'NONE',  ( -0.000000000000000000, -0.000000000000000000, 1.000000000000000000 ) ) ;
#4943 = CARTESIAN_POINT ( 'NONE',  ( 27.70933665152130132, 40.41277845351218190, 11.00000000000000000 ) ) ;
#4944 = AXIS2_PLACEMENT_3D ( 'NONE', #1312, #6676, #1192 ) ;
#4945 = CIRCLE ( 'NONE', #6093, 5.000000000000007994 ) ;
#4946 = CARTESIAN_POINT ( 'NONE',  ( 1.999999999999994449, -45.00000000000000000, 23.99999999999999645 ) ) ;
#4947 = ORIENTED_EDGE ( 'NONE', *, *, #22126, .T. ) ;
#4948 = DIRECTION ( 'NONE',  ( 0.000000000000000000, -1.000000000000000000, 0.000000000000000000 ) ) ;
#4949 = CARTESIAN_POINT ( 'NONE',  ( -34.00000000000000000, 3.999999999999999112, 9.500000000000000000 ) ) ;
#4950 = CARTESIAN_POINT ( 'NONE',  ( 9.500000000000000000, 6.470877716354879437E-13, -4.059589141758143782 ) ) ;
#4951 = VECTOR ( 'NONE', #20876, 1000.000000000000000 ) ;
#4952 = DIRECTION ( 'NONE',  ( -1.000000000000000000, 0.000000000000000000, 0.000000000000000000 ) ) ;
#4953 = CIRCLE ( 'NONE', #8027, 4.250000000000000000 ) ;
#4954 = ORIENTED_EDGE ( 'NONE', *, *, #241, .T. ) ;
#4955 = EDGE_LOOP ( 'NONE', ( #7820, #6022, #23962, #17042, #4736 ) ) ;
#4956 = ORIENTED_EDGE ( 'NONE', *, *, #16147, .F. ) ;
#4957 = ORIENTED_EDGE ( 'NONE', *, *, #13088, .F. ) ;
#4958 = CARTESIAN_POINT ( 'NONE',  ( 34.02499999999999858, 29.50000000000000000, -3.000000000000000000 ) ) ;
#4959 = EDGE_CURVE ( 'NONE', #13970, #11339, #13916, .T. ) ;
#4960 = AXIS2_PLACEMENT_3D ( 'NONE', #8098, #9647, #11111 ) ;
#4961 = ORIENTED_EDGE ( 'NONE', *, *, #8172, .F. ) ;
#4962 = FACE_OUTER_BOUND ( 'NONE', #23430, .T. ) ;
#4963 = DIRECTION ( 'NONE',  ( 0.000000000000000000, 0.000000000000000000, 1.000000000000000000 ) ) ;
#4964 = DIRECTION ( 'NONE',  ( 0.000000000000000000, 0.000000000000000000, 1.000000000000000000 ) ) ;
#4965 = EDGE_CURVE ( 'NONE', #13594, #3962, #19258, .T. ) ;
#4966 = CARTESIAN_POINT ( 'NONE',  ( 6.999999999999999112, 0.000000000000000000, 0.000000000000000000 ) ) ;
#4967 = EDGE_LOOP ( 'NONE', ( #22817, #9798, #3210, #5662 ) ) ;
#4968 = DIRECTION ( 'NONE',  ( -1.000000000000000000, 0.000000000000000000, -0.000000000000000000 ) ) ;
#4969 = DIRECTION ( 'NONE',  ( -0.000000000000000000, -0.000000000000000000, -1.000000000000000000 ) ) ;
#4970 = EDGE_CURVE ( 'NONE', #16756, #3463, #10291, .T. ) ;
#4971 = CARTESIAN_POINT ( 'NONE',  ( 41.49999999999999289, 27.79189783386526358, 27.00000000000000000 ) ) ;
#4972 = B_SPLINE_CURVE_WITH_KNOTS ( 'NONE', 3,
 ( #16990, #8559, #21135, #17475, #4934, #10403, #15627, #15774, #14064, #8320, #6386, #892, #21276, #13690, #1257, #13829, #17858, #6514, #23238, #11972, #8678, #10509, #6745, #12086, #21510, #19443 ),
 .UNSPECIFIED., .F., .F.,
 ( 4, 2, 2, 2, 2, 2, 2, 2, 2, 2, 2, 2, 4 ),
 ( 0.006142831834825534729, 0.008468238795519878598, 0.01079364575621422247, 0.01195634923656139527, 0.01311905271690856807, 0.01428175619725574087, 0.01544445967760291367, 0.01660716315795008474, 0.01776986663829725754, 0.01893257011864443035, 0.02009527359899160315, 0.02242068055968594181, 0.02474608752038028742 ),
 .UNSPECIFIED. ) ;
#4973 = LINE ( 'NONE', #14212, #22980 ) ;
#4974 = DIRECTION ( 'NONE',  ( -0.000000000000000000, -0.000000000000000000, -1.000000000000000000 ) ) ;
#4975 = CARTESIAN_POINT ( 'NONE',  ( 41.73082370883260239, 50.99999999999999289, 0.000000000000000000 ) ) ;
#4976 = DIRECTION ( 'NONE',  ( 1.000000000000000000, 0.000000000000000000, 0.000000000000000000 ) ) ;
#4977 = CARTESIAN_POINT ( 'NONE',  ( -5.622572944242077574E-13, 8.680847955711007202, -3.133165578109187610 ) ) ;
#4978 = ORIENTED_EDGE ( 'NONE', *, *, #16378, .T. ) ;
#4979 = CARTESIAN_POINT ( 'NONE',  ( -31.10231664966676846, 45.36128193761570770, 12.00000000000000000 ) ) ;
#4980 = ORIENTED_EDGE ( 'NONE', *, *, #7590, .T. ) ;
#4981 = CARTESIAN_POINT ( 'NONE',  ( -6.233975306307046963E-13, 9.127583699786111282, 5.133165578109188054 ) ) ;
#4982 = PRODUCT ( 'Part11^Assembly Idle gear', 'Part11^Assembly Idle gear', '', ( #1783 ) ) ;
#4983 = DIRECTION ( 'NONE',  ( -0.000000000000000000, -0.000000000000000000, -1.000000000000000000 ) ) ;
#4984 = ORIENTED_EDGE ( 'NONE', *, *, #4431, .T. ) ;
#4985 = ORIENTED_EDGE ( 'NONE', *, *, #19701, .F. ) ;
#4986 = CARTESIAN_POINT ( 'NONE',  ( -6.249999999999999112, -10.82531754730548279, 2.500000000000000000 ) ) ;
#4987 = CARTESIAN_POINT ( 'NONE',  ( -7.685661446562381371, 5.583959896777970222, -4.859589141758143604 ) ) ;
#4988 = CARTESIAN_POINT ( 'NONE',  ( -6.153822176767817416E-13, 9.500000000000000000, 3.186529713919380669 ) ) ;
#4989 = CARTESIAN_POINT ( 'NONE',  ( 3.373806935227752118E-18, 0.000000000000000000, 0.000000000000000000 ) ) ;
#4990 = CARTESIAN_POINT ( 'NONE',  ( 23.00000000000000000, -6.393861490227931377, 9.782270569456429143 ) ) ;
#4991 = EDGE_CURVE ( 'NONE', #1599, #1413, #4395, .T. ) ;
#4992 = ADVANCED_FACE ( 'NONE', ( #23188 ), #17552, .T. ) ;
#4993 = VERTEX_POINT ( 'NONE', #19150 ) ;
#4994 = DIRECTION ( 'NONE',  ( -0.000000000000000000, -0.000000000000000000, -1.000000000000000000 ) ) ;
#4995 = CYLINDRICAL_SURFACE ( 'NONE', #967, 6.050000000006051870 ) ;
#4996 = ORIENTED_EDGE ( 'NONE', *, *, #5507, .F. ) ;
#4997 = CARTESIAN_POINT ( 'NONE',  ( 5.078177448618334644, 0.000000000000000000, 11.24716442891539714 ) ) ;
#4998 = ORIENTED_EDGE ( 'NONE', *, *, #815, .T. ) ;
#4999 = CARTESIAN_POINT ( 'NONE',  ( -21.84999999999999787, 16.67999999999984695, 13.00000000000000178 ) ) ;
#5000 = CARTESIAN_POINT ( 'NONE',  ( 0.000000000000000000, 0.000000000000000000, 15.50000000000000000 ) ) ;
#5001 = DIRECTION ( 'NONE',  ( 0.000000000000000000, 0.000000000000000000, -1.000000000000000000 ) ) ;
#5002 = ORIENTED_EDGE ( 'NONE', *, *, #14086, .T. ) ;
#5003 = CYLINDRICAL_SURFACE ( 'NONE', #16075, 5.000000000000000888 ) ;
#5004 = ORIENTED_EDGE ( 'NONE', *, *, #18930, .T. ) ;
#5005 = ORIENTED_EDGE ( 'NONE', *, *, #8731, .T. ) ;
#5006 = CARTESIAN_POINT ( 'NONE',  ( 9.500000000000000000, 6.470877716354879437E-13, 6.059589141758143782 ) ) ;
#5007 = CARTESIAN_POINT ( 'NONE',  ( -5.871322893124554021, 8.081182679343978492, 5.906742014460233392 ) ) ;
#5008 = CARTESIAN_POINT ( 'NONE',  ( 41.99999999999999289, 5.618459588085056979E-15, 0.000000000000000000 ) ) ;
#5009 = PRODUCT_DEFINITION ( 'UNKNOWN', '', #9971, #4250 ) ;
#5010 = CIRCLE ( 'NONE', #15087, 5.000000000000007994 ) ;
#5011 = VERTEX_POINT ( 'NONE', #15479 ) ;
#5012 =( LENGTH_UNIT ( ) NAMED_UNIT ( * ) SI_UNIT ( .MILLI., .METRE. ) );
#5013 = EDGE_CURVE ( 'NONE', #10964, #581, #19283, .T. ) ;
#5014 = DIRECTION ( 'NONE',  ( -1.000000000000000000, -0.000000000000000000, -0.000000000000000000 ) ) ;
#5015 = LINE ( 'NONE', #17822, #13081 ) ;
#5016 = CARTESIAN_POINT ( 'NONE',  ( -9.500000000000000000, -6.482511860946779655E-13, -4.206742014460233214 ) ) ;
#5017 = ADVANCED_FACE ( 'NONE', ( #4164 ), #12952, .F. ) ;
#5018 = FILL_AREA_STYLE ('',( #17827 ) ) ;
#5019 = CARTESIAN_POINT ( 'NONE',  ( -29.00000000000000000, -29.49999999999999645, 12.00000000000000000 ) ) ;
#5020 = EDGE_CURVE ( 'NONE', #1863, #1766, #15754, .T. ) ;
#5021 = EDGE_CURVE ( 'NONE', #23953, #11737, #20046, .T. ) ;
#5022 = ADVANCED_FACE ( 'NONE', ( #6001 ), #14569, .F. ) ;
#5023 = ORIENTED_EDGE ( 'NONE', *, *, #16836, .F. ) ;
#5024 = ORIENTED_EDGE ( 'NONE', *, *, #16355, .F. ) ;
#5025 = CARTESIAN_POINT ( 'NONE',  ( 70.21613547800127719, -5.000000000000000888, 6.123233995736776143E-16 ) ) ;
#5026 = DIRECTION ( 'NONE',  ( -1.000000000000000000, -1.224606353822377258E-16, -0.000000000000000000 ) ) ;
#5027 = DIRECTION ( 'NONE',  ( 0.000000000000000000, -1.000000000000000000, -0.000000000000000000 ) ) ;
#5028 = AXIS2_PLACEMENT_3D ( 'NONE', #20281, #11098, #14535 ) ;
#5029 = DIRECTION ( 'NONE',  ( 0.000000000000000000, 0.000000000000000000, -1.000000000000000000 ) ) ;
#5030 = ORIENTED_EDGE ( 'NONE', *, *, #13782, .T. ) ;
#5031 = CARTESIAN_POINT ( 'NONE',  ( -14.99999999999999822, -6.045577542124163753E-21, 9.499999999999994671 ) ) ;
#5032 = ORIENTED_EDGE ( 'NONE', *, *, #789, .F. ) ;
#5033 = ORIENTED_EDGE ( 'NONE', *, *, #2996, .T. ) ;
#5034 = CARTESIAN_POINT ( 'NONE',  ( -8.680847955711200825, 2.820578480813073607, 3.533165578109187965 ) ) ;
#5035 = DIRECTION ( 'NONE',  ( -0.000000000000000000, -0.000000000000000000, -1.000000000000000000 ) ) ;
#5036 = CLOSED_SHELL ( 'NONE', ( #13881, #16282, #16849, #10644, #19462, #6342, #2525, #8672, #7591, #10012, #12466, #21170, #22092, #16089, #19678, #10253, #10115, #12375, #17953, #23814, #110, #8776, #20949, #4876, #21471, #14510, #9542, #3611, #7948, #13480, #15856, #3205, #18271, #20591, #16503, #14327, #20663, #4181, #14607, #7650, #11968, #11469, #4992, #17095, #21837, #8541, #20050, #14896, #2838, #17523, #6658, #2768 ) ) ;
#5037 = ORIENTED_EDGE ( 'NONE', *, *, #16308, .T. ) ;
#5038 = CARTESIAN_POINT ( 'NONE',  ( 8.840695694414906214, -0.6121865488562178159, -12.50000000000000000 ) ) ;
#5039 = EDGE_CURVE ( 'NONE', #20363, #18828, #15239, .T. ) ;
#5040 = CYLINDRICAL_SURFACE ( 'NONE', #8252, 15.00000000000000000 ) ;
#5041 = DIRECTION ( 'NONE',  ( -0.000000000000000000, -0.000000000000000000, -1.000000000000000000 ) ) ;
#5042 = EDGE_LOOP ( 'NONE', ( #21825, #7512, #21129, #7227, #8370 ) ) ;
#5043 = EDGE_CURVE ( 'NONE', #17472, #15489, #22175, .T. ) ;
#5044 = FACE_OUTER_BOUND ( 'NONE', #7608, .T. ) ;
#5045 = ADVANCED_FACE ( 'NONE', ( #21621 ), #17709, .F. ) ;
#5046 = CARTESIAN_POINT ( 'NONE',  ( -6.822232771736903637E-13, 9.988891130263535700, -7.706742014460232326 ) ) ;
#5047 = ORIENTED_EDGE ( 'NONE', *, *, #15234, .T. ) ;
#5048 = ORIENTED_EDGE ( 'NONE', *, *, #18882, .T. ) ;
#5049 = CARTESIAN_POINT ( 'NONE',  ( -41.50000000000000000, -28.80990663662250739, 11.00000000000000000 ) ) ;
#5050 = DIRECTION ( 'NONE',  ( 0.000000000000000000, 0.000000000000000000, -1.000000000000000000 ) ) ;
#5051 = ORIENTED_EDGE ( 'NONE', *, *, #7004, .F. ) ;
#5052 = DIRECTION ( 'NONE',  ( -1.000000000000000000, -0.000000000000000000, -0.000000000000000000 ) ) ;
#5053 = DIRECTION ( 'NONE',  ( 1.000000000000000000, 0.000000000000000000, 0.000000000000000000 ) ) ;
#5054 = ORIENTED_EDGE ( 'NONE', *, *, #16845, .F. ) ;
#5055 = CARTESIAN_POINT ( 'NONE',  ( -41.99999999999997158, -25.22443390181683043, -3.000000000000000000 ) ) ;
#5056 = DIRECTION ( 'NONE',  ( 0.000000000000000000, 0.000000000000000000, -1.000000000000000000 ) ) ;
#5057 = CARTESIAN_POINT ( 'NONE',  ( 7.685661446561619314, 5.583959896779020049, -4.259589141758143960 ) ) ;
#5058 = LINE ( 'NONE', #13927, #6697 ) ;
#5059 = ORIENTED_EDGE ( 'NONE', *, *, #7611, .T. ) ;
#5060 = AXIS2_PLACEMENT_3D ( 'NONE', #3473, #3117, #10889 ) ;
#5061 = ORIENTED_EDGE ( 'NONE', *, *, #14442, .F. ) ;
#5062 = CARTESIAN_POINT ( 'NONE',  ( -0.9830802669677229932, 45.00000000000000000, 3.000000000000002665 ) ) ;
#5063 = ADVANCED_FACE ( 'NONE', ( #8793 ), #6010, .F. ) ;
#5064 = CARTESIAN_POINT ( 'NONE',  ( 3.890962118697714531E-15, 15.50000000000000000, 7.700000000000001954 ) ) ;
#5065 = DIRECTION ( 'NONE',  ( 1.000000000000000000, 0.000000000000000000, 0.000000000000000000 ) ) ;
#5066 = VERTEX_POINT ( 'NONE', #23452 ) ;
#5067 = DIRECTION ( 'NONE',  ( -0.000000000000000000, -0.000000000000000000, -1.000000000000000000 ) ) ;
#5068 = DIRECTION ( 'NONE',  ( 1.000000000000000000, -4.625929269271481378E-15, 0.000000000000000000 ) ) ;
#5069 = ORIENTED_EDGE ( 'NONE', *, *, #17306, .F. ) ;
#5070 = CARTESIAN_POINT ( 'NONE',  ( 7.685661446562381371, -5.583959896777971110, -9.006742014460233037 ) ) ;
#5071 = CARTESIAN_POINT ( 'NONE',  ( 7.685661446561619314, 5.583959896779020049, 5.406742014460233392 ) ) ;
#5072 = CARTESIAN_POINT ( 'NONE',  ( -2.935661446561384391, -9.035036904804158553, 4.606742014460233570 ) ) ;
#5073 = DIRECTION ( 'NONE',  ( -0.000000000000000000, -0.000000000000000000, -1.000000000000000000 ) ) ;
#5074 = LINE ( 'NONE', #14096, #61 ) ;
#5075 = AXIS2_PLACEMENT_3D ( 'NONE', #17703, #10246, #21252 ) ;
#5076 = CARTESIAN_POINT ( 'NONE',  ( 23.00000000000000000, 0.000000000000000000, 0.000000000000000000 ) ) ;
#5077 = CARTESIAN_POINT ( 'NONE',  ( 8.680847955711007202, 5.912916378492122225E-13, -4.633165578109188942 ) ) ;
#5078 = ADVANCED_FACE ( 'NONE', ( #14506 ), #21743, .T. ) ;
#5079 = CARTESIAN_POINT ( 'NONE',  ( 70.21613547800127719, 7.562528597612068045E-15, 0.000000000000000000 ) ) ;
#5080 = VERTEX_POINT ( 'NONE', #6727 ) ;
#5081 = EDGE_CURVE ( 'NONE', #19097, #14695, #6427, .T. ) ;
#5082 = DIRECTION ( 'NONE',  ( 1.000000000000000000, 0.000000000000000000, -0.000000000000000000 ) ) ;
#5083 = ORIENTED_EDGE ( 'NONE', *, *, #399, .T. ) ;
#5084 = EDGE_CURVE ( 'NONE', #3894, #5686, #10383, .T. ) ;
#5085 = B_SPLINE_CURVE_WITH_KNOTS ( 'NONE', 3,
 ( #12516, #19988, #22296, #5461, #10696, #5222, #14727, #16206, #22189, #12414, #1463, #1565, #10571, #12651, #5099, #20118, #1336, #16422, #20230, #3147, #18166, #3394, #8872, #16313, #10917, #9696, #16911, #6064, #20835, #11399, #11272, #4117, #13010, #22781, #9335, #5932 ),
 .UNSPECIFIED., .F., .F.,
 ( 4, 2, 2, 2, 2, 2, 2, 2, 2, 2, 2, 2, 2, 2, 2, 2, 2, 4 ),
 ( 8.673617379884035472E-19, 0.002901772246161930194, 0.003627215307702410033, 0.004352658369242889437, 0.005803544492323848246, 0.006528987553864327650, 0.007254430615404807922, 0.008705316738485763262, 0.01015620286156672034, 0.01160708898464767394, 0.01305797510772863101, 0.01450886123080958809, 0.01595974735389054516, 0.01741063347697149877, 0.01886151960005245237, 0.02031240572313340598, 0.02176329184621436305, 0.02321417796929531666 ),
 .UNSPECIFIED. ) ;
#5086 = CARTESIAN_POINT ( 'NONE',  ( 73.12522638709218370, 5.000000000000015987, 0.000000000000000000 ) ) ;
#5087 = CARTESIAN_POINT ( 'NONE',  ( -7.685661446562381371, 5.583959896777970222, -6.859589141758143604 ) ) ;
#5088 = CARTESIAN_POINT ( 'NONE',  ( 5.000000000000000000, 2.342598717236902939, -4.057500000000001883 ) ) ;
#5089 = CYLINDRICAL_SURFACE ( 'NONE', #2980, 11.22592346138681130 ) ;
#5090 = CARTESIAN_POINT ( 'NONE',  ( 41.00000000000000000, 26.23076770084981746, 12.00000000000000000 ) ) ;
#5091 = AXIS2_PLACEMENT_3D ( 'NONE', #11856, #21398, #17729 ) ;
#5092 = DIRECTION ( 'NONE',  ( 0.000000000000000000, 0.000000000000000000, -1.000000000000000000 ) ) ;
#5093 = CARTESIAN_POINT ( 'NONE',  ( 0.000000000000000000, 10.59264252385243665, -4.936618945406485714 ) ) ;
#5094 = ORIENTED_EDGE ( 'NONE', *, *, #21027, .F. ) ;
#5095 = CARTESIAN_POINT ( 'NONE',  ( -9.000000000000000000, 1.102182119232617714E-15, 0.9999999999999940048 ) ) ;
#5096 = VERTEX_POINT ( 'NONE', #17956 ) ;
#5097 = CARTESIAN_POINT ( 'NONE',  ( 86.51113724927145654, 7.420530141404717394E-15, 0.000000000000000000 ) ) ;
#5098 = DIRECTION ( 'NONE',  ( 0.000000000000000000, -0.8660254037844390407, -0.4999999999999993339 ) ) ;
#5099 = CARTESIAN_POINT ( 'NONE',  ( 17.38700629636781869, 8.908123924593985166, 3.336041480784317503 ) ) ;
#5100 = LINE ( 'NONE', #5348, #23559 ) ;
#5101 = VERTEX_POINT ( 'NONE', #3310 ) ;
#5102 = DIRECTION ( 'NONE',  ( -0.000000000000000000, -0.000000000000000000, 1.000000000000000000 ) ) ;
#5103 = EDGE_CURVE ( 'NONE', #8450, #15532, #6824, .T. ) ;
#5104 = CARTESIAN_POINT ( 'NONE',  ( 29.00000000000000000, -29.50000000000000355, 12.00000000000000000 ) ) ;
#5105 = ORIENTED_EDGE ( 'NONE', *, *, #4157, .T. ) ;
#5106 = EDGE_LOOP ( 'NONE', ( #15566, #20870, #6329, #23357, #18968 ) ) ;
#5107 = CARTESIAN_POINT ( 'NONE',  ( 5.871322893124553133, -8.081182679343980269, 5.759589141758144848 ) ) ;
#5108 = ADVANCED_FACE ( 'NONE', ( #17842 ), #5261, .F. ) ;
#5109 = CARTESIAN_POINT ( 'NONE',  ( 5.871322893123449127, 8.081182679344781405, 9.506742014460231260 ) ) ;
#5110 = EDGE_CURVE ( 'NONE', #598, #20174, #3073, .T. ) ;
#5111 = VERTEX_POINT ( 'NONE', #16115 ) ;
#5112 = CARTESIAN_POINT ( 'NONE',  ( 28.99999999999998579, -29.49999999999999645, -3.000000000000000000 ) ) ;
#5113 = DIRECTION ( 'NONE',  ( -0.000000000000000000, -0.000000000000000000, -1.000000000000000000 ) ) ;
#5114 = CARTESIAN_POINT ( 'NONE',  ( 0.000000000000000000, 0.000000000000000000, -3.000000000000000000 ) ) ;
#5115 = DIRECTION ( 'NONE',  ( 1.000000000000000000, -0.000000000000000000, -0.000000000000000000 ) ) ;
#5116 = CARTESIAN_POINT ( 'NONE',  ( 76.90909090909090651, 4.172000000000015696, 0.000000000000000000 ) ) ;
#5117 = CARTESIAN_POINT ( 'NONE',  ( 20.85000000000000497, 16.67999999999999972, 14.50000000000000000 ) ) ;
#5118 = AXIS2_PLACEMENT_3D ( 'NONE', #16372, #14191, #12594 ) ;
#5119 =( REPRESENTATION_RELATIONSHIP ('NONE','NONE', #21748, #2851 ) REPRESENTATION_RELATIONSHIP_WITH_TRANSFORMATION ( #19069 )SHAPE_REPRESENTATION_RELATIONSHIP( ) );
#5120 = EDGE_LOOP ( 'NONE', ( #15275, #22815, #12477, #5023 ) ) ;
#5121 = SURFACE_SIDE_STYLE ('',( #10835 ) ) ;
#5122 = CARTESIAN_POINT ( 'NONE',  ( -6.822232771736904647E-13, 9.988891130263535700, 10.55958914175814201 ) ) ;
#5123 = COLOUR_RGB ( '',0.7921568627450980005, 0.8196078431372548767, 0.9333333333333333481 ) ;
#5124 = CARTESIAN_POINT ( 'NONE',  ( -10.49999999999999822, 1.285879139104720633E-15, -3.499999999999999556 ) ) ;
#5125 = CARTESIAN_POINT ( 'NONE',  ( -5.976739099259236459E-13, 9.226949318570335734, -3.515549869009883643 ) ) ;
#5126 = DIRECTION ( 'NONE',  ( 1.000000000000000000, 0.000000000000000000, 0.000000000000000000 ) ) ;
#5127 = CARTESIAN_POINT ( 'NONE',  ( 9.000000000000000000, 1.102182119232617714E-15, 0.4999999999999970024 ) ) ;
#5128 = EDGE_LOOP ( 'NONE', ( #20065, #6190 ) ) ;
#5129 = DIRECTION ( 'NONE',  ( -1.000000000000000000, -0.000000000000000000, -0.000000000000000000 ) ) ;
#5130 = ORIENTED_EDGE ( 'NONE', *, *, #22164, .T. ) ;
#5131 = CARTESIAN_POINT ( 'NONE',  ( 0.000000000000000000, -2.342598717236905603, 4.057500000000010765 ) ) ;
#5132 = EDGE_CURVE ( 'NONE', #21270, #2607, #22793, .T. ) ;
#5133 = CARTESIAN_POINT ( 'NONE',  ( -14.51962751333974033, -3.765689428759031010, 27.00000000000000000 ) ) ;
#5134 = VECTOR ( 'NONE', #11719, 1000.000000000000000 ) ;
#5135 = EDGE_CURVE ( 'NONE', #9659, #18218, #14676, .T. ) ;
#5136 = ORIENTED_EDGE ( 'NONE', *, *, #16561, .F. ) ;
#5137 = CARTESIAN_POINT ( 'NONE',  ( 8.511897654723162177, -2.099402067127676297, -12.50000000000000000 ) ) ;
#5138 = DIRECTION ( 'NONE',  ( -1.000000000000000000, -0.000000000000000000, -0.000000000000000000 ) ) ;
#5139 = AXIS2_PLACEMENT_3D ( 'NONE', #19269, #4521, #13901 ) ;
#5140 = CIRCLE ( 'NONE', #18764, 5.000000000000007994 ) ;
#5141 = FACE_OUTER_BOUND ( 'NONE', #13926, .T. ) ;
#5142 = AXIS2_PLACEMENT_3D ( 'NONE', #9409, #304, #21145 ) ;
#5143 = ORIENTED_EDGE ( 'NONE', *, *, #18379, .T. ) ;
#5144 = FACE_OUTER_BOUND ( 'NONE', #21466, .T. ) ;
#5145 = DIRECTION ( 'NONE',  ( -1.000000000000000000, -1.224606353822377258E-16, -0.000000000000000000 ) ) ;
#5146 = CARTESIAN_POINT ( 'NONE',  ( -6.153822176767817416E-13, 9.500000000000000000, -3.706742014460232326 ) ) ;
#5147 = VERTEX_POINT ( 'NONE', #1009 ) ;
#5148 = ORIENTED_EDGE ( 'NONE', *, *, #12510, .F. ) ;
#5149 = DIRECTION ( 'NONE',  ( -1.000000000000000000, 0.000000000000000000, 0.000000000000000000 ) ) ;
#5150 = EDGE_CURVE ( 'NONE', #3844, #4495, #10604, .T. ) ;
#5151 = CONICAL_SURFACE ( 'NONE', #6314, 4.172000000000008590, 0.9599310885968742602 ) ;
#5152 = AXIS2_PLACEMENT_3D ( 'NONE', #4284, #629, #5986 ) ;
#5153 = AXIS2_PLACEMENT_3D ( 'NONE', #371, #9496, #3904 ) ;
#5154 = ORIENTED_EDGE ( 'NONE', *, *, #11206, .F. ) ;
#5155 = CONICAL_SURFACE ( 'NONE', #5550, 5.000000000000007994, 0.9599310885968855844 ) ;
#5156 = PRODUCT_DEFINITION_SHAPE ( 'NONE', 'NONE',  #22438 ) ;
#5157 = CARTESIAN_POINT ( 'NONE',  ( 0.000000000000000000, 0.000000000000000000, 105.0000000000000000 ) ) ;
#5158 = CONICAL_SURFACE ( 'NONE', #14872, 5.000000000000007994, 0.9599310885968855844 ) ;
#5159 = DIRECTION ( 'NONE',  ( -0.000000000000000000, -0.000000000000000000, -1.000000000000000000 ) ) ;
#5160 = VERTEX_POINT ( 'NONE', #6613 ) ;
#5161 = AXIS2_PLACEMENT_3D ( 'NONE', #19683, #1245, #2957 ) ;
#5162 = DIRECTION ( 'NONE',  ( -1.000000000000000000, -0.000000000000000000, -0.000000000000000000 ) ) ;
#5163 = CARTESIAN_POINT ( 'NONE',  ( -29.00000000000000000, 29.50000000000000000, 16.55365763086713216 ) ) ;
#5164 = EDGE_CURVE ( 'NONE', #21270, #430, #15366, .T. ) ;
#5165 = CARTESIAN_POINT ( 'NONE',  ( -1.504652183083727168, 9.499999999999904077, -3.757996296007079184 ) ) ;
#5166 = ADVANCED_FACE ( 'NONE', ( #9260 ), #258, .T. ) ;
#5167 = DIRECTION ( 'NONE',  ( -0.000000000000000000, -0.000000000000000000, -1.000000000000000000 ) ) ;
#5168 = VERTEX_POINT ( 'NONE', #3541 ) ;
#5169 = ORIENTED_EDGE ( 'NONE', *, *, #12371, .T. ) ;
#5170 = CIRCLE ( 'NONE', #7131, 4.999999999999997335 ) ;
#5171 = ORIENTED_EDGE ( 'NONE', *, *, #15125, .F. ) ;
#5172 = VECTOR ( 'NONE', #16713, 1000.000000000000000 ) ;
#5174 = VECTOR ( 'NONE', #18548, 1000.000000000000000 ) ;
#5173 = DIRECTION ( 'NONE',  ( -0.000000000000000000, -0.000000000000000000, -1.000000000000000000 ) ) ;
#5175 = VECTOR ( 'NONE', #14268, 1000.000000000000000 ) ;
#5176 = CIRCLE ( 'NONE', #15283, 11.68650000001168543 ) ;
#5177 = CARTESIAN_POINT ( 'NONE',  ( 71.67068093254673045, -5.000000000000000888, 6.123233995736776143E-16 ) ) ;
#5178 = CARTESIAN_POINT ( 'NONE',  ( -39.00000000000000000, 0.000000000000000000, 11.00000000000000000 ) ) ;
#5179 = ORIENTED_EDGE ( 'NONE', *, *, #22529, .T. ) ;
#5180 = ORIENTED_EDGE ( 'NONE', *, *, #17847, .T. ) ;
#5181 = FACE_OUTER_BOUND ( 'NONE', #9786, .T. ) ;
#5182 = DIRECTION ( 'NONE',  ( 1.000000000000000000, 0.000000000000000000, 0.000000000000000000 ) ) ;
#5183 = CARTESIAN_POINT ( 'NONE',  ( -5.871322893124554021, 8.081182679343978492, 3.906742014460231616 ) ) ;
#5184 = CARTESIAN_POINT ( 'NONE',  ( 29.00000000000000000, 29.50000000000000355, 11.50000000000000000 ) ) ;
#5185 = DIRECTION ( 'NONE',  ( 0.000000000000000000, 0.000000000000000000, -1.000000000000000000 ) ) ;
#5186 = CYLINDRICAL_SURFACE ( 'NONE', #18158, 6.050000000006050982 ) ;
#5187 = AXIS2_PLACEMENT_3D ( 'NONE', #14434, #16830, #20751 ) ;
#5188 = DIRECTION ( 'NONE',  ( 1.000000000000000000, 0.000000000000000000, 0.000000000000000000 ) ) ;
#5189 = DIRECTION ( 'NONE',  ( 0.7052211081716904806, 0.7089874389501500396, 0.000000000000000000 ) ) ;
#5190 = CARTESIAN_POINT ( 'NONE',  ( 86.21613547800127719, 5.000000000000015099, 0.000000000000000000 ) ) ;
#5191 = ADVANCED_FACE ( 'NONE', ( #14756 ), #3898, .T. ) ;
#5192 = CIRCLE ( 'NONE', #14536, 3.000000000000002665 ) ;
#5193 = EDGE_CURVE ( 'NONE', #11499, #11436, #20063, .T. ) ;
#5194 = CARTESIAN_POINT ( 'NONE',  ( 8.680847955711007202, 5.912916378492122225E-13, 10.63316557810918894 ) ) ;
#5195 = VERTEX_POINT ( 'NONE', #22565 ) ;
#5196 = AXIS2_PLACEMENT_3D ( 'NONE', #2986, #14073, #14542 ) ;
#5197 = AXIS2_PLACEMENT_3D ( 'NONE', #9984, #20992, #6220 ) ;
#5198 = CARTESIAN_POINT ( 'NONE',  ( 664.7818939062880190, 917.9837211537981148, 1368.981724745927977 ) ) ;
#5199 = DIRECTION ( 'NONE',  ( 0.000000000000000000, -1.000000000000000000, 0.000000000000000000 ) ) ;
#5200 = ORIENTED_EDGE ( 'NONE', *, *, #12853, .F. ) ;
#5201 = VERTEX_POINT ( 'NONE', #14987 ) ;
#5202 = DIRECTION ( 'NONE',  ( 0.000000000000000000, 0.000000000000000000, 1.000000000000000000 ) ) ;
#5203 = CARTESIAN_POINT ( 'NONE',  ( -6.822232771736903637E-13, 9.988891130263535700, -8.559589141758145558 ) ) ;
#5204 = LINE ( 'NONE', #5561, #12225 ) ;
#5206 = AXIS2_PLACEMENT_3D ( 'NONE', #8785, #1487, #23333 ) ;
#5205 = CARTESIAN_POINT ( 'NONE',  ( -30.31394790604173295, -39.41330121100982353, 11.00000000000000000 ) ) ;
#5207 = DIRECTION ( 'NONE',  ( 1.000000000000000000, 0.000000000000000000, -0.000000000000000000 ) ) ;
#5208 = CIRCLE ( 'NONE', #21972, 5.100000000000000533 ) ;
#5209 = DIRECTION ( 'NONE',  ( -1.000000000000000000, -0.000000000000000000, 0.000000000000000000 ) ) ;
#5210 = VERTEX_POINT ( 'NONE', #18774 ) ;
#5211 = CIRCLE ( 'NONE', #23531, 3.500000000000003109 ) ;
#5212 = DIRECTION ( 'NONE',  ( -0.7071067811865474617, 0.000000000000000000, -0.7071067811865474617 ) ) ;
#5213 = CIRCLE ( 'NONE', #7157, 9.725923461386811297 ) ;
#5214 = ADVANCED_FACE ( 'NONE', ( #9015 ), #14209, .T. ) ;
#5215 = VECTOR ( 'NONE', #12852, 1000.000000000000000 ) ;
#5216 = ORIENTED_EDGE ( 'NONE', *, *, #22673, .T. ) ;
#5217 = DIRECTION ( 'NONE',  ( -0.7071067811865469066, 8.659560562354926695E-17, 0.7071067811865482389 ) ) ;
#5218 = VERTEX_POINT ( 'NONE', #14645 ) ;
#5219 = CARTESIAN_POINT ( 'NONE',  ( -14.99999999999999645, 15.50000000000000178, 7.700000000000001954 ) ) ;
#5220 = CIRCLE ( 'NONE', #7525, 6.050000000006051870 ) ;
#5221 = CARTESIAN_POINT ( 'NONE',  ( -42.00000000000000000, 25.22443390181683043, -3.000000000000000000 ) ) ;
#5222 = CARTESIAN_POINT ( 'NONE',  ( 16.36153765883235423, 6.593687918952694460, 6.842832175870693590 ) ) ;
#5223 = CIRCLE ( 'NONE', #23935, 0.2999999999999999334 ) ;
#5224 = ADVANCED_FACE ( 'NONE', ( #9486 ), #22464, .F. ) ;
#5225 = FACE_OUTER_BOUND ( 'NONE', #18860, .T. ) ;
#5226 = ORIENTED_EDGE ( 'NONE', *, *, #894, .T. ) ;
#5227 = DIRECTION ( 'NONE',  ( -0.5735764363510517105, -0.8191520442889879128, 0.000000000000000000 ) ) ;
#5228 = EDGE_CURVE ( 'NONE', #23675, #14561, #11075, .T. ) ;
#5229 = DIRECTION ( 'NONE',  ( 0.000000000000000000, 0.000000000000000000, 1.000000000000000000 ) ) ;
#5230 = ORIENTED_EDGE ( 'NONE', *, *, #7984, .T. ) ;
#5231 = ORIENTED_EDGE ( 'NONE', *, *, #294, .T. ) ;
#5232 = CARTESIAN_POINT ( 'NONE',  ( 9.500000000000209610, -3.086737114211962396, 9.106742014460232681 ) ) ;
#5233 = CARTESIAN_POINT ( 'NONE',  ( 9.500000000000209610, -3.086737114211962396, 5.106742014460234458 ) ) ;
#5234 = DIRECTION ( 'NONE',  ( -0.000000000000000000, -0.000000000000000000, -1.000000000000000000 ) ) ;
#5235 = VERTEX_POINT ( 'NONE', #7319 ) ;
#5236 = ORIENTED_EDGE ( 'NONE', *, *, #535, .T. ) ;
#5237 = DIRECTION ( 'NONE',  ( -8.033660851157631600E-27, 9.483094156888088166E-28, 1.000000000000000000 ) ) ;
#5238 = CIRCLE ( 'NONE', #4065, 9.747164428915397139 ) ;
#5239 = CARTESIAN_POINT ( 'NONE',  ( 79.81818181818181301, 4.172000000000015696, 0.000000000000000000 ) ) ;
#5240 = CARTESIAN_POINT ( 'NONE',  ( 61.78386452199871570, 7.420530141404717394E-15, 0.000000000000000000 ) ) ;
#5241 = CIRCLE ( 'NONE', #21999, 5.000000000000007994 ) ;
#5242 = CARTESIAN_POINT ( 'NONE',  ( 41.99999999999999289, 6.904644888889564703E-15, 10.50249999999999950 ) ) ;
#5243 = AXIS2_PLACEMENT_3D ( 'NONE', #1530, #10775, #18240 ) ;
#5244 = VECTOR ( 'NONE', #7846, 1000.000000000000000 ) ;
#5245 = CIRCLE ( 'NONE', #17710, 4.499999999999997335 ) ;
#5246 = CARTESIAN_POINT ( 'NONE',  ( 0.000000000000000000, -15.03999999999999915, -25.00000000000000000 ) ) ;
#5247 = CARTESIAN_POINT ( 'NONE',  ( 71.67068093254673045, 7.562528597612068045E-15, 0.000000000000000000 ) ) ;
#5248 = EDGE_CURVE ( 'NONE', #23000, #16942, #2062, .T. ) ;
#5249 = ORIENTED_EDGE ( 'NONE', *, *, #13555, .F. ) ;
#5250 = EDGE_CURVE ( 'NONE', #20068, #14422, #22016, .T. ) ;
#5251 = LINE ( 'NONE', #22105, #11709 ) ;
#5252 = CARTESIAN_POINT ( 'NONE',  ( 9.499999999999790390, 3.086737114213260025, 10.15958914175814343 ) ) ;
#5253 = CARTESIAN_POINT ( 'NONE',  ( -1.253758815873204258, 9.437348638249524413, -3.501083568643978960 ) ) ;
#5254 = CARTESIAN_POINT ( 'NONE',  ( 7.685661446562381371, -5.583959896777971110, -11.85958914175814449 ) ) ;
#5255 = VECTOR ( 'NONE', #3721, 1000.000000000000114 ) ;
#5256 = CARTESIAN_POINT ( 'NONE',  ( -41.99999999999999289, 0.000000000000000000, 0.000000000000000000 ) ) ;
#5257 = CARTESIAN_POINT ( 'NONE',  ( -2.682529543900285862, 8.255977015246234174, -9.233165578109188587 ) ) ;
#5258 = AXIS2_PLACEMENT_3D ( 'NONE', #4257, #17535, #5757 ) ;
#5259 = CARTESIAN_POINT ( 'NONE',  ( -45.00000000000001421, 50.99999999999992184, 12.50000000000000000 ) ) ;
#5260 = ORIENTED_EDGE ( 'NONE', *, *, #16902, .T. ) ;
#5261 = CYLINDRICAL_SURFACE ( 'NONE', #11453, 4.999999999999997335 ) ;
#5262 = ORIENTED_EDGE ( 'NONE', *, *, #22910, .F. ) ;
#5263 = DIRECTION ( 'NONE',  ( 0.000000000000000000, 0.000000000000000000, 1.000000000000000000 ) ) ;
#5264 = FACE_OUTER_BOUND ( 'NONE', #796, .T. ) ;
#5265 = ORIENTED_EDGE ( 'NONE', *, *, #11902, .T. ) ;
#5266 = CARTESIAN_POINT ( 'NONE',  ( 8.871028110654306076, 6.042456644462176420E-13, -12.50000000000000000 ) ) ;
#5267 = CIRCLE ( 'NONE', #6437, 9.500000000000000000 ) ;
#5268 = DIRECTION ( 'NONE',  ( -0.000000000000000000, -0.000000000000000000, -1.000000000000000000 ) ) ;
#5269 = DIRECTION ( 'NONE',  ( -1.000000000000000000, -0.000000000000000000, -0.000000000000000000 ) ) ;
#5270 = DIRECTION ( 'NONE',  ( 0.000000000000000000, 0.000000000000000000, 1.000000000000000000 ) ) ;
#5271 = ORIENTED_EDGE ( 'NONE', *, *, #2941, .T. ) ;
#5272 = APPLICATION_CONTEXT ( 'automotive_design' ) ;
#5273 = DIRECTION ( 'NONE',  ( 0.7052211081716915908, -0.7089874389501490404, 0.000000000000000000 ) ) ;
#5274 = VECTOR ( 'NONE', #3934, 1000.000000000000114 ) ;
#5275 = CARTESIAN_POINT ( 'NONE',  ( 9.500000000000000000, 6.470877716354879437E-13, -5.206742014460234103 ) ) ;
#5276 = ORIENTED_EDGE ( 'NONE', *, *, #4465, .F. ) ;
#5277 = CIRCLE ( 'NONE', #985, 10.00000000000000888 ) ;
#5278 = EDGE_LOOP ( 'NONE', ( #20804, #4193, #10154, #841 ) ) ;
#5279 = CARTESIAN_POINT ( 'NONE',  ( -6.153822176767817416E-13, 9.500000000000000000, -3.706742014460231882 ) ) ;
#5280 = ADVANCED_FACE ( 'NONE', ( #5743 ), #18560, .F. ) ;
#5281 = EDGE_CURVE ( 'NONE', #16706, #8325, #12805, .T. ) ;
#5282 = CIRCLE ( 'NONE', #18915, 4.499999999999997335 ) ;
#5283 = DIRECTION ( 'NONE',  ( -1.000000000000000000, 0.000000000000000000, 0.000000000000000000 ) ) ;
#5284 = CARTESIAN_POINT ( 'NONE',  ( 87.96568270381690979, 7.420530141404717394E-15, 0.000000000000000000 ) ) ;
#5285 = VECTOR ( 'NONE', #13805, 1000.000000000000000 ) ;
#5286 = ORIENTED_EDGE ( 'NONE', *, *, #23686, .T. ) ;
#5287 = DIRECTION ( 'NONE',  ( 0.000000000000000000, 0.000000000000000000, 1.000000000000000000 ) ) ;
#5288 = CARTESIAN_POINT ( 'NONE',  ( 14.94708199919714531, -1.300481340138138098, 9.416259293296516120 ) ) ;
#5289 = DIRECTION ( 'NONE',  ( 1.000000000000000000, 0.000000000000000000, 0.000000000000000000 ) ) ;
#5290 = ORIENTED_EDGE ( 'NONE', *, *, #5281, .F. ) ;
#5291 = CARTESIAN_POINT ( 'NONE',  ( 66.72727272727273373, 7.491529369508391930E-15, 0.000000000000000000 ) ) ;
#5292 = CARTESIAN_POINT ( 'NONE',  ( 3.890962118697714531E-15, 15.50000000000000000, -2.999999999999999112 ) ) ;
#5293 = CARTESIAN_POINT ( 'NONE',  ( 14.51962751333974389, -3.765689428759035895, -27.00000000000000000 ) ) ;
#5294 = AXIS2_PLACEMENT_3D ( 'NONE', #18093, #23232, #17722 ) ;
#5295 = CARTESIAN_POINT ( 'NONE',  ( 0.000000000000000000, 0.000000000000000000, 0.000000000000000000 ) ) ;
#5296 = CONICAL_SURFACE ( 'NONE', #16959, 2.024999999999999911, 0.7853981633974222998 ) ;
#5297 = ORIENTED_EDGE ( 'NONE', *, *, #10265, .F. ) ;
#5298 = ORIENTED_EDGE ( 'NONE', *, *, #299, .T. ) ;
#5299 = AXIS2_PLACEMENT_3D ( 'NONE', #20566, #10785, #16528 ) ;
#5300 = EDGE_CURVE ( 'NONE', #13710, #831, #15765, .T. ) ;
#5301 = VERTEX_POINT ( 'NONE', #1595 ) ;
#5302 = ORIENTED_EDGE ( 'NONE', *, *, #12606, .F. ) ;
#5303 = CARTESIAN_POINT ( 'NONE',  ( 3.890962118697714531E-15, 15.50000000000000000, 7.700000000000001954 ) ) ;
#5304 = ADVANCED_FACE ( 'NONE', ( #7418 ), #13820, .T. ) ;
#5305 = FACE_OUTER_BOUND ( 'NONE', #14551, .T. ) ;
#5306 = VERTEX_POINT ( 'NONE', #129 ) ;
#5307 = VERTEX_POINT ( 'NONE', #1718 ) ;
#5308 = EDGE_CURVE ( 'NONE', #5096, #3802, #24042, .T. ) ;
#5309 = EDGE_CURVE ( 'NONE', #2171, #18698, #23961, .T. ) ;
#5310 = CIRCLE ( 'NONE', #21281, 6.050000000006052758 ) ;
#5311 = EDGE_CURVE ( 'NONE', #23953, #10776, #17064, .T. ) ;
#5312 = FACE_OUTER_BOUND ( 'NONE', #19220, .T. ) ;
#5313 = ORIENTED_EDGE ( 'NONE', *, *, #18473, .F. ) ;
#5314 = AXIS2_PLACEMENT_3D ( 'NONE', #6801, #10551, #14340 ) ;
#5316 = CARTESIAN_POINT ( 'NONE',  ( -8.585126421212056158, 3.981676010260311482, 12.03996617712741646 ) ) ;
#5315 = VECTOR ( 'NONE', #112, 1000.000000000000000 ) ;
#5317 = DIRECTION ( 'NONE',  ( -0.000000000000000000, -0.000000000000000000, 1.000000000000000000 ) ) ;
#5318 = CARTESIAN_POINT ( 'NONE',  ( 0.000000000000000000, 0.000000000000000000, 0.000000000000000000 ) ) ;
#5319 = CARTESIAN_POINT ( 'NONE',  ( -45.00000000000001421, 50.99999999999992184, 12.50000000000000000 ) ) ;
#5320 = VECTOR ( 'NONE', #20138, 1000.000000000000227 ) ;
#5321 = CARTESIAN_POINT ( 'NONE',  ( -40.00000000000000000, 28.80990663662251450, 0.000000000000000000 ) ) ;
#5322 = DIRECTION ( 'NONE',  ( 0.000000000000000000, 1.000000000000000000, 0.000000000000000000 ) ) ;
#5323 = DIRECTION ( 'NONE',  ( 0.000000000000000000, -1.000000000000000000, 0.000000000000000000 ) ) ;
#5324 = EDGE_LOOP ( 'NONE', ( #18369, #994, #8295, #17309 ) ) ;
#5325 = CARTESIAN_POINT ( 'NONE',  ( -8.680847955710813579, -2.820578480814258437, 11.73316557810918859 ) ) ;
#5326 = ORIENTED_EDGE ( 'NONE', *, *, #7673, .F. ) ;
#5327 = ADVANCED_FACE ( 'NONE', ( #18911 ), #2194, .F. ) ;
#5328 = DIRECTION ( 'NONE',  ( -0.5735764363510517105, -0.8191520442889879128, 0.000000000000000000 ) ) ;
#5329 = VECTOR ( 'NONE', #17881, 1000.000000000000000 ) ;
#5330 = ORIENTED_EDGE ( 'NONE', *, *, #15913, .T. ) ;
#5331 = ORIENTED_EDGE ( 'NONE', *, *, #2709, .F. ) ;
#5332 = CARTESIAN_POINT ( 'NONE',  ( 0.000000000000000000, 0.000000000000000000, 0.9999999999999940048 ) ) ;
#5333 = CARTESIAN_POINT ( 'NONE',  ( 2.935661446561383503, 9.035036904804158553, -8.459589141758144137 ) ) ;
#5334 = TOROIDAL_SURFACE ( 'NONE', #23983, 51.49999999999999289, 1.500000000000000000 ) ;
#5335 = EDGE_CURVE ( 'NONE', #1240, #5235, #11133, .T. ) ;
#5336 = CARTESIAN_POINT ( 'NONE',  ( -39.99999999999999289, 15.50000000000000000, 19.20000000000000995 ) ) ;
#5337 = CARTESIAN_POINT ( 'NONE',  ( -28.27483331787890819, -41.23752903419608629, -27.00000000000000000 ) ) ;
#5338 = CARTESIAN_POINT ( 'NONE',  ( -40.77574956473004164, -27.49633847812775755, 12.00000000000000000 ) ) ;
#5339 = ADVANCED_FACE ( 'NONE', ( #15270 ), #18973, .T. ) ;
#5340 = CARTESIAN_POINT ( 'NONE',  ( 0.000000000000000000, 45.00000000000000000, -27.00000000000000000 ) ) ;
#5341 = ORIENTED_EDGE ( 'NONE', *, *, #22832, .F. ) ;
#5342 = CARTESIAN_POINT ( 'NONE',  ( 70.21613547800127719, 5.000000000000015987, 0.000000000000000000 ) ) ;
#5343 = CIRCLE ( 'NONE', #18984, 4.172000000000008590 ) ;
#5344 = CARTESIAN_POINT ( 'NONE',  ( 29.00000000000000000, 29.50000000000000355, 11.50000000000000000 ) ) ;
#5345 = DIRECTION ( 'NONE',  ( 0.000000000000000000, -1.000000000000000000, 0.000000000000000000 ) ) ;
#5346 = DIRECTION ( 'NONE',  ( 0.000000000000000000, 0.000000000000000000, 1.000000000000000000 ) ) ;
#5347 = ORIENTED_EDGE ( 'NONE', *, *, #7304, .F. ) ;
#5348 = CARTESIAN_POINT ( 'NONE',  ( -2.983080266967717442, 45.00000000000000000, 3.000000000000002665 ) ) ;
#5349 = CARTESIAN_POINT ( 'NONE',  ( 58.00000000000000000, -4.172000000000000597, 0.000000000000000000 ) ) ;
#5350 = SHAPE_REPRESENTATION ( 'Assembly Idle gear', ( #5695, #23994, #13466 ), #22456 ) ;
#5351 = DIRECTION ( 'NONE',  ( 0.000000000000000000, 0.000000000000000000, 1.000000000000000000 ) ) ;
#5352 = ORIENTED_EDGE ( 'NONE', *, *, #19495, .F. ) ;
#5353 = ORIENTED_EDGE ( 'NONE', *, *, #2100, .T. ) ;
#5354 = CARTESIAN_POINT ( 'NONE',  ( 5.871322893124553133, -8.081182679343980269, 10.90674201446023339 ) ) ;
#5355 = CARTESIAN_POINT ( 'NONE',  ( 7.685661446562381371, -5.583959896777971110, 7.006742014460233037 ) ) ;
#5356 = DIRECTION ( 'NONE',  ( 0.000000000000000000, 0.000000000000000000, 1.000000000000000000 ) ) ;
#5357 = ORIENTED_EDGE ( 'NONE', *, *, #20017, .T. ) ;
#5358 = ORIENTED_EDGE ( 'NONE', *, *, #12429, .F. ) ;
#5359 = DIRECTION ( 'NONE',  ( 0.9999999999999998890, 4.282024058902498337E-31, 3.944304526105059027E-31 ) ) ;
#5360 = DIRECTION ( 'NONE',  ( 1.000000000000000000, 0.000000000000000000, -0.000000000000000000 ) ) ;
#5361 = CARTESIAN_POINT ( 'NONE',  ( 3.530011532367169913, 0.000000000000000000, 0.000000000000000000 ) ) ;
#5362 = CYLINDRICAL_SURFACE ( 'NONE', #20071, 11.68650000001168721 ) ;
#5363 = CARTESIAN_POINT ( 'NONE',  ( 5.871322893124551356, -8.081182679343980269, -4.906742014460232504 ) ) ;
#5364 = CARTESIAN_POINT ( 'NONE',  ( 77.48886275072855767, 7.562528597612068045E-15, 0.000000000000000000 ) ) ;
#5365 = FILL_AREA_STYLE ('',( #11178 ) ) ;
#5366 = DIRECTION ( 'NONE',  ( -1.000000000000000000, -0.000000000000000000, -0.000000000000000000 ) ) ;
#5367 = EDGE_CURVE ( 'NONE', #3750, #12835, #7825, .T. ) ;
#5368 = ORIENTED_EDGE ( 'NONE', *, *, #5043, .T. ) ;
#5369 = PRODUCT_DEFINITION_SHAPE ( 'NONE', 'NONE',  #24127 ) ;
#5370 = CARTESIAN_POINT ( 'NONE',  ( -29.00000000000000000, -3.851859888774471706E-31, 11.00000000000000000 ) ) ;
#5371 = VERTEX_POINT ( 'NONE', #18839 ) ;
#5372 = DIRECTION ( 'NONE',  ( 0.000000000000000000, 0.000000000000000000, 1.000000000000000000 ) ) ;
#5373 = CYLINDRICAL_SURFACE ( 'NONE', #16504, 1.500000000000001332 ) ;
#5374 = TOROIDAL_SURFACE ( 'NONE', #19011, 12.73082370883260062, 1.500000000000000000 ) ;
#5375 = DIRECTION ( 'NONE',  ( -1.000000000000000000, -1.224606353822377258E-16, -0.000000000000000000 ) ) ;
#5376 = DIRECTION ( 'NONE',  ( -1.000000000000000000, 0.000000000000000000, 0.000000000000000000 ) ) ;
#5377 = LINE ( 'NONE', #20498, #6646 ) ;
#5378 = CARTESIAN_POINT ( 'NONE',  ( 6.222797240145152671E-13, -9.127583699786111282, -10.13316557810918894 ) ) ;
#5379 = AXIS2_PLACEMENT_3D ( 'NONE', #18267, #16415, #23998 ) ;
#5380 = CARTESIAN_POINT ( 'NONE',  ( 0.000000000000000000, 0.000000000000000000, 3.499999999999999556 ) ) ;
#5381 = AXIS2_PLACEMENT_3D ( 'NONE', #19923, #6750, #6518 ) ;
#5382 = EDGE_LOOP ( 'NONE', ( #3805, #1920, #18954, #8393 ) ) ;
#5383 = CARTESIAN_POINT ( 'NONE',  ( 6.250000000000000000, 10.82531754730548279, 2.500000000000000000 ) ) ;
#5384 = EDGE_LOOP ( 'NONE', ( #13171, #14563, #1331, #17832 ) ) ;
#5385 = CARTESIAN_POINT ( 'NONE',  ( 1.999999999999994449, 45.00000000000000000, 26.97499999999999432 ) ) ;
#5386 = EDGE_CURVE ( 'NONE', #14839, #20691, #9505, .T. ) ;
#5387 = ORIENTED_EDGE ( 'NONE', *, *, #18930, .F. ) ;
#5388 = CARTESIAN_POINT ( 'NONE',  ( -9.500000000000000000, 0.000000000000000000, 12.50000000000000000 ) ) ;
#5389 = CARTESIAN_POINT ( 'NONE',  ( 0.000000000000000000, 0.000000000000000000, 0.000000000000000000 ) ) ;
#5390 = DIRECTION ( 'NONE',  ( -1.000000000000000000, -0.000000000000000000, -0.000000000000000000 ) ) ;
#5391 = EDGE_CURVE ( 'NONE', #21092, #6327, #8360, .T. ) ;
#5392 = FACE_OUTER_BOUND ( 'NONE', #913, .T. ) ;
#5393 = DIRECTION ( 'NONE',  ( 0.000000000000000000, 0.000000000000000000, -1.000000000000000000 ) ) ;
#5394 = CIRCLE ( 'NONE', #19037, 1.000000000000000888 ) ;
#5395 = CARTESIAN_POINT ( 'NONE',  ( 9.500000000000209610, -3.086737114211962396, -7.959589141758143249 ) ) ;
#5396 = VERTEX_POINT ( 'NONE', #5677 ) ;
#5397 = ORIENTED_EDGE ( 'NONE', *, *, #12498, .F. ) ;
#5398 = CYLINDRICAL_SURFACE ( 'NONE', #19263, 9.999999999999998224 ) ;
#5399 = DIRECTION ( 'NONE',  ( -0.000000000000000000, -0.000000000000000000, 1.000000000000000000 ) ) ;
#5400 = DIRECTION ( 'NONE',  ( -0.000000000000000000, -0.000000000000000000, -1.000000000000000000 ) ) ;
#5401 = FILL_AREA_STYLE ('',( #1959 ) ) ;
#5402 = VERTEX_POINT ( 'NONE', #7467 ) ;
#5403 = CIRCLE ( 'NONE', #11608, 5.000000000000007994 ) ;
#5404 = DIRECTION ( 'NONE',  ( -1.000000000000000000, 0.000000000000000000, -0.000000000000000000 ) ) ;
#5405 = CARTESIAN_POINT ( 'NONE',  ( 29.00000000000000711, -29.50000000000000711, -27.00000000000000000 ) ) ;
#5406 = DIRECTION ( 'NONE',  ( 1.000000000000000000, -1.776356839400250465E-15, 0.000000000000000000 ) ) ;
#5407 = ORIENTED_EDGE ( 'NONE', *, *, #3127, .T. ) ;
#5408 = CARTESIAN_POINT ( 'NONE',  ( 11.50000000000000000, -7.812991839788874238, 16.07708877602009068 ) ) ;
#5409 = CARTESIAN_POINT ( 'NONE',  ( -23.84999999999999432, -15.03999999999999915, -25.00000000000000000 ) ) ;
#5410 = DIRECTION ( 'NONE',  ( -1.000000000000000000, 0.000000000000000000, 0.000000000000000000 ) ) ;
#5411 = CARTESIAN_POINT ( 'NONE',  ( -7.022953521755574080, 5.102474405759713783, 3.433165578109189209 ) ) ;
#5412 = ORIENTED_EDGE ( 'NONE', *, *, #4262, .F. ) ;
#5413 = EDGE_CURVE ( 'NONE', #15778, #2345, #16748, .T. ) ;
#5414 = EDGE_LOOP ( 'NONE', ( #7539, #18217, #20096, #15248 ) ) ;
#5415 = ADVANCED_FACE ( 'NONE', ( #15150 ), #19688, .T. ) ;
#5416 = VERTEX_POINT ( 'NONE', #3836 ) ;
#5417 = ORIENTED_EDGE ( 'NONE', *, *, #23762, .T. ) ;
#5418 = ORIENTED_EDGE ( 'NONE', *, *, #10368, .T. ) ;
#5419 = DIRECTION ( 'NONE',  ( 4.613626265895764052E-16, -1.000000000000000000, 0.000000000000000000 ) ) ;
#5420 = CARTESIAN_POINT ( 'NONE',  ( 0.000000000000000000, 45.00000000000000000, 27.00000000000000000 ) ) ;
#5421 = ORIENTED_EDGE ( 'NONE', *, *, #20354, .T. ) ;
#5422 = VERTEX_POINT ( 'NONE', #13469 ) ;
#5423 = CARTESIAN_POINT ( 'NONE',  ( 42.00000000000000000, 25.22443390181681622, -3.000000000000000000 ) ) ;
#5424 = DIRECTION ( 'NONE',  ( 0.000000000000000000, -1.000000000000000000, 0.000000000000000000 ) ) ;
#5425 = ORIENTED_EDGE ( 'NONE', *, *, #4287, .T. ) ;
#5426 = CARTESIAN_POINT ( 'NONE',  ( 7.999999999999986677, 9.797174393178809880E-16, 53.00000000000000000 ) ) ;
#5427 = DIRECTION ( 'NONE',  ( 0.000000000000000000, 0.000000000000000000, -1.000000000000000000 ) ) ;
#5428 = CARTESIAN_POINT ( 'NONE',  ( 5.871322893124551356, -8.081182679343980269, 10.90674201446023339 ) ) ;
#5429 = CARTESIAN_POINT ( 'NONE',  ( -39.99999999999999289, -29.50000000000001066, 27.00000000000000000 ) ) ;
#5430 = DIRECTION ( 'NONE',  ( -0.000000000000000000, -0.000000000000000000, -1.000000000000000000 ) ) ;
#5431 = EDGE_CURVE ( 'NONE', #11173, #15649, #5901, .T. ) ;
#5432 = DIRECTION ( 'NONE',  ( 0.000000000000000000, -0.7071067811865536790, -0.7071067811865414665 ) ) ;
#5433 = FACE_OUTER_BOUND ( 'NONE', #3430, .T. ) ;
#5434 = CARTESIAN_POINT ( 'NONE',  ( -1.999999999999996669, -45.00000000000000000, -8.673617379884035472E-16 ) ) ;
#5435 = EDGE_CURVE ( 'NONE', #5851, #17470, #5541, .T. ) ;
#5436 = ORIENTED_EDGE ( 'NONE', *, *, #15696, .F. ) ;
#5437 = CARTESIAN_POINT ( 'NONE',  ( 8.680847955711199049, -2.820578480813074496, 8.533165578109187521 ) ) ;
#5438 = ORIENTED_EDGE ( 'NONE', *, *, #20665, .T. ) ;
#5439 = AXIS2_PLACEMENT_3D ( 'NONE', #8106, #15550, #8361 ) ;
#5440 = EDGE_CURVE ( 'NONE', #3497, #1636, #22394, .T. ) ;
#5441 = ADVANCED_FACE ( 'NONE', ( #1774, #417, #9413, #18483, #9203, #7363 ), #2123, .T. ) ;
#5442 = APPLICATION_PROTOCOL_DEFINITION ( 'draft international standard', 'automotive_design', 1998, #5272 ) ;
#5443 = CARTESIAN_POINT ( 'NONE',  ( -31.74999999999995737, 0.000000000000000000, 0.000000000000000000 ) ) ;
#5444 = VERTEX_POINT ( 'NONE', #22264 ) ;
#5445 = ORIENTED_EDGE ( 'NONE', *, *, #8108, .T. ) ;
#5446 = DIRECTION ( 'NONE',  ( -0.5735764363510517105, -0.8191520442889879128, 0.000000000000000000 ) ) ;
#5447 = CARTESIAN_POINT ( 'NONE',  ( -8.680847955711007202, -5.923547351154968927E-13, -11.63316557810919072 ) ) ;
#5448 = EDGE_LOOP ( 'NONE', ( #5793, #14925, #7705, #68 ) ) ;
#5449 = CARTESIAN_POINT ( 'NONE',  ( -6.153822176767817416E-13, 9.500000000000000000, 3.706742014460231882 ) ) ;
#5450 = CARTESIAN_POINT ( 'NONE',  ( 79.23840997654417606, 7.420530141404717394E-15, 0.000000000000000000 ) ) ;
#5451 = DIRECTION ( 'NONE',  ( 1.000000000000000000, 0.000000000000000000, 0.000000000000000000 ) ) ;
#5452 = DIRECTION ( 'NONE',  ( 1.000000000000000000, 0.000000000000000000, 0.000000000000000000 ) ) ;
#5453 = VECTOR ( 'NONE', #5328, 1000.000000000000000 ) ;
#5454 = ORIENTED_EDGE ( 'NONE', *, *, #9462, .F. ) ;
#5455 = DIRECTION ( 'NONE',  ( -1.000000000000000000, 0.000000000000000000, 0.000000000000000000 ) ) ;
#5456 = ORIENTED_EDGE ( 'NONE', *, *, #13561, .F. ) ;
#5457 = VECTOR ( 'NONE', #18307, 1000.000000000000000 ) ;
#5458 = DIRECTION ( 'NONE',  ( -0.8757121056631640421, 0.4828336235133042775, -0.000000000000000000 ) ) ;
#5459 = LINE ( 'NONE', #12880, #7810 ) ;
#5460 = LINE ( 'NONE', #14954, #6764 ) ;
#5461 = CARTESIAN_POINT ( 'NONE',  ( 16.08510323282435195, 6.088885580147183063, 7.295537496892087859 ) ) ;
#5462 = EDGE_CURVE ( 'NONE', #19051, #17352, #22619, .T. ) ;
#5463 = EDGE_CURVE ( 'NONE', #11221, #5671, #14962, .T. ) ;
#5464 = FACE_OUTER_BOUND ( 'NONE', #10215, .T. ) ;
#5465 = CARTESIAN_POINT ( 'NONE',  ( 67.30704456891035647, 7.562528597612068045E-15, 0.000000000000000000 ) ) ;
#5466 = PRESENTATION_STYLE_ASSIGNMENT (( #16559 ) ) ;
#5467 = ORIENTED_EDGE ( 'NONE', *, *, #5812, .F. ) ;
#5468 = VERTEX_POINT ( 'NONE', #7596 ) ;
#5469 = CARTESIAN_POINT ( 'NONE',  ( 7.685661446561619314, 5.583959896779020049, 7.406742014460233392 ) ) ;
#5470 = EDGE_CURVE ( 'NONE', #17358, #11482, #15043, .T. ) ;
#5471 = ORIENTED_EDGE ( 'NONE', *, *, #10572, .F. ) ;
#5472 = EDGE_CURVE ( 'NONE', #7070, #16945, #17004, .T. ) ;
#5473 = EDGE_LOOP ( 'NONE', ( #5880, #8960, #19584, #10040 ) ) ;
#5474 = CARTESIAN_POINT ( 'NONE',  ( -23.85000000000000142, 15.03999999999999737, 2.200000000000000178 ) ) ;
#5475 = AXIS2_PLACEMENT_3D ( 'NONE', #7932, #10005, #11841 ) ;
#5476 = FACE_OUTER_BOUND ( 'NONE', #20842, .T. ) ;
#5477 = LINE ( 'NONE', #20355, #10259 ) ;
#5478 = DIRECTION ( 'NONE',  ( 1.000000000000000000, 0.000000000000000000, 0.000000000000000000 ) ) ;
#5479 = CARTESIAN_POINT ( 'NONE',  ( 2.024999999999999911, 45.00000000000000000, 27.00000000000000000 ) ) ;
#5480 = ORIENTED_EDGE ( 'NONE', *, *, #18683, .F. ) ;
#5481 = LINE ( 'NONE', #16701, #9005 ) ;
#5482 =( NAMED_UNIT ( * ) SI_UNIT ( $, .STERADIAN. ) SOLID_ANGLE_UNIT ( ) );
#5483 = CARTESIAN_POINT ( 'NONE',  ( -9.499999999999962697, -8.297908579805900909E-07, -3.500254135480583617 ) ) ;
#5484 = CARTESIAN_POINT ( 'NONE',  ( 83.60204634018053582, 7.420530141404717394E-15, 0.000000000000000000 ) ) ;
#5485 =( BOUNDED_CURVE ( )  B_SPLINE_CURVE ( 2, ( #17308, #13647, #7894, #16805, #2420, #4015, #21085, #9845, #19033, #17173, #609 ),
 .UNSPECIFIED., .F., .T. ) 
 B_SPLINE_CURVE_WITH_KNOTS ( ( 3, 2, 2, 2, 2, 3 ),
 ( 0.8000000000000000444, 0.8199999999999999512, 0.8399999999999999689, 0.8599999999999999867, 0.8800000000000000044, 0.9000000000000000222 ),
 .UNSPECIFIED. ) 
 CURVE ( )  GEOMETRIC_REPRESENTATION_ITEM ( )  RATIONAL_B_SPLINE_CURVE ( ( 1.000000000000000000, 0.9510565162951535312, 1.000000000000000000, 0.9510565162951535312, 1.000000000000000000, 0.9510565162951535312, 1.000000000000000000, 0.9510565162951535312, 1.000000000000000000, 0.9510565162951535312, 1.000000000000000000 ) ) 
 REPRESENTATION_ITEM ( '' )  );
#5486 = CARTESIAN_POINT ( 'NONE',  ( 29.00000000000000000, 29.50000000000000000, -3.000000000000000000 ) ) ;
#5487 = DIRECTION ( 'NONE',  ( -0.8571673007021120005, 0.000000000000000000, -0.5150380749100547106 ) ) ;
#5488 = ORIENTED_EDGE ( 'NONE', *, *, #12262, .F. ) ;
#5489 = DIRECTION ( 'NONE',  ( 0.000000000000000000, 0.000000000000000000, 1.000000000000000000 ) ) ;
#5490 = VERTEX_POINT ( 'NONE', #22990 ) ;
#5491 = CARTESIAN_POINT ( 'NONE',  ( -36.00000000000000711, -51.00000000000000711, 12.50000000000000000 ) ) ;
#5492 = DIRECTION ( 'NONE',  ( -1.000000000000000000, 0.000000000000000000, 0.000000000000000000 ) ) ;
#5493 = EDGE_CURVE ( 'NONE', #13107, #18342, #19204, .T. ) ;
#5494 = EDGE_LOOP ( 'NONE', ( #9504, #21215, #4764, #10518 ) ) ;
#5495 = EDGE_CURVE ( 'NONE', #22890, #20318, #13962, .T. ) ;
#5496 = CARTESIAN_POINT ( 'NONE',  ( 57.42022815836235594, 6.123233995736675563E-16, -5.000000000000007994 ) ) ;
#5497 = CARTESIAN_POINT ( 'NONE',  ( 80.39795365981946418, 7.562528597612068045E-15, 0.000000000000000000 ) ) ;
#5498 = DIRECTION ( 'NONE',  ( -0.000000000000000000, -0.000000000000000000, -1.000000000000000000 ) ) ;
#5499 = AXIS2_PLACEMENT_3D ( 'NONE', #23018, #4488, #572 ) ;
#5500 = CARTESIAN_POINT ( 'NONE',  ( 9.500000000000000000, 6.470877716354879437E-13, -10.05958914175814378 ) ) ;
#5501 = ORIENTED_EDGE ( 'NONE', *, *, #19524, .F. ) ;
#5502 = ORIENTED_EDGE ( 'NONE', *, *, #17877, .T. ) ;
#5503 = CARTESIAN_POINT ( 'NONE',  ( -2.999999999999999112, 6.000000000000000000, 80.99999999999998579 ) ) ;
#5504 = EDGE_CURVE ( 'NONE', #21975, #8445, #15409, .T. ) ;
#5505 = ORIENTED_EDGE ( 'NONE', *, *, #17891, .T. ) ;
#5506 = DIRECTION ( 'NONE',  ( 0.000000000000000000, -0.000000000000000000, -1.000000000000000000 ) ) ;
#5507 = EDGE_CURVE ( 'NONE', #2834, #7627, #15782, .T. ) ;
#5508 = EDGE_LOOP ( 'NONE', ( #20554, #16548, #12842, #22397 ) ) ;
#5509 = CARTESIAN_POINT ( 'NONE',  ( 10.00000000000000000, 0.000000000000000000, 0.000000000000000000 ) ) ;
#5510 = DIRECTION ( 'NONE',  ( -1.000000000000000000, 0.000000000000000000, 0.000000000000000000 ) ) ;
#5511 = DIRECTION ( 'NONE',  ( -0.000000000000000000, -1.000000000000000000, -0.000000000000000000 ) ) ;
#5512 = AXIS2_PLACEMENT_3D ( 'NONE', #7235, #14675, #4952 ) ;
#5513 = ORIENTED_EDGE ( 'NONE', *, *, #11087, .F. ) ;
#5514 = CARTESIAN_POINT ( 'NONE',  ( 0.000000000000000000, 0.000000000000000000, 12.50000000000000000 ) ) ;
#5515 = EDGE_CURVE ( 'NONE', #14903, #9833, #19292, .T. ) ;
#5516 = CARTESIAN_POINT ( 'NONE',  ( 7.022953521755574080, -5.102474405759714671, 12.43316557810918788 ) ) ;
#5517 = CIRCLE ( 'NONE', #21103, 1.499999999999998002 ) ;
#5518 = DIRECTION ( 'NONE',  ( -1.000000000000000000, 0.000000000000000000, -0.000000000000000000 ) ) ;
#5519 = VECTOR ( 'NONE', #12743, 1000.000000000000000 ) ;
#5520 = CARTESIAN_POINT ( 'NONE',  ( -5.365059087799947335, 7.384370330706355290, 5.333165578109189120 ) ) ;
#5521 = EDGE_LOOP ( 'NONE', ( #21574, #11368 ) ) ;
#5522 = ORIENTED_EDGE ( 'NONE', *, *, #18001, .T. ) ;
#5523 = VERTEX_POINT ( 'NONE', #19451 ) ;
#5524 = ORIENTED_EDGE ( 'NONE', *, *, #3647, .F. ) ;
#5525 = DIRECTION ( 'NONE',  ( 1.000000000000000000, 0.000000000000000000, 0.000000000000000000 ) ) ;
#5526 = CARTESIAN_POINT ( 'NONE',  ( 7.685661446561619314, 5.583959896779020049, 9.406742014460235168 ) ) ;
#5527 = ORIENTED_EDGE ( 'NONE', *, *, #7793, .T. ) ;
#5528 = CONICAL_SURFACE ( 'NONE', #14105, 9.500000000000000000, 0.7853981633974500554 ) ;
#5529 = EDGE_LOOP ( 'NONE', ( #16448, #19368, #2118, #5330 ) ) ;
#5530 = AXIS2_PLACEMENT_3D ( 'NONE', #15737, #23199, #7786 ) ;
#5531 = EDGE_CURVE ( 'NONE', #16881, #7962, #12095, .T. ) ;
#5532 = CARTESIAN_POINT ( 'NONE',  ( 87.67068093254673045, 5.000000000000015987, 0.000000000000000000 ) ) ;
#5533 = AXIS2_PLACEMENT_3D ( 'NONE', #8073, #15519, #4689 ) ;
#5534 = ORIENTED_EDGE ( 'NONE', *, *, #1808, .F. ) ;
#5535 = CARTESIAN_POINT ( 'NONE',  ( -37.00000000000000711, -29.49999999999999645, 11.50000000000000000 ) ) ;
#5536 = CIRCLE ( 'NONE', #11352, 40.00000000000000000 ) ;
#5537 = EDGE_CURVE ( 'NONE', #6271, #19427, #16169, .T. ) ;
#5538 = DIRECTION ( 'NONE',  ( -0.7071067811865456854, 0.000000000000000000, -0.7071067811865493491 ) ) ;
#5539 = DIRECTION ( 'NONE',  ( 0.000000000000000000, -0.000000000000000000, -1.000000000000000000 ) ) ;
#5540 = PLANE ( 'NONE',  #15394 ) ;
#5541 = LINE ( 'NONE', #11498, #2923 ) ;
#5542 = CARTESIAN_POINT ( 'NONE',  ( 0.000000000000000000, 0.000000000000000000, 0.000000000000000000 ) ) ;
#5543 = CARTESIAN_POINT ( 'NONE',  ( 5.000000000000000000, -2.342598717236905603, 4.057500000000010765 ) ) ;
#5544 = CARTESIAN_POINT ( 'NONE',  ( -14.94777716362147935, 1.291632522116891391, -9.417361603030281358 ) ) ;
#5545 = ORIENTED_EDGE ( 'NONE', *, *, #988, .F. ) ;
#5546 = CARTESIAN_POINT ( 'NONE',  ( -2.682529543899159208, -8.255977015246598327, 10.03316557810918930 ) ) ;
#5547 = VERTEX_POINT ( 'NONE', #11867 ) ;
#5548 = AXIS2_PLACEMENT_3D ( 'NONE', #2018, #7990, #5811 ) ;
#5549 = VECTOR ( 'NONE', #15996, 1000.000000000000000 ) ;
#5550 = AXIS2_PLACEMENT_3D ( 'NONE', #6459, #13399, #2553 ) ;
#5551 = SHAPE_DEFINITION_REPRESENTATION ( #3206, #17018 ) ;
#5552 = AXIS2_PLACEMENT_3D ( 'NONE', #5509, #22590, #17202 ) ;
#5553 = CIRCLE ( 'NONE', #12947, 10.00000000000000533 ) ;
#5554 = ORIENTED_EDGE ( 'NONE', *, *, #5470, .F. ) ;
#5555 = ORIENTED_EDGE ( 'NONE', *, *, #10199, .F. ) ;
#5556 = PRODUCT_DEFINITION_SHAPE ( 'NONE', 'NONE',  #24116 ) ;
#5557 = DIRECTION ( 'NONE',  ( 0.000000000000000000, 0.5000000000000013323, 0.8660254037844379305 ) ) ;
#5558 = CARTESIAN_POINT ( 'NONE',  ( -5.365059087799947335, 7.384370330706355290, -9.333165578109190008 ) ) ;
#5559 = AXIS2_PLACEMENT_3D ( 'NONE', #10619, #922, #19466 ) ;
#5560 = VERTEX_POINT ( 'NONE', #8331 ) ;
#5561 = CARTESIAN_POINT ( 'NONE',  ( 84.18181818181818699, 4.172000000000015696, 5.109226446042767468E-16 ) ) ;
#5562 = CYLINDRICAL_SURFACE ( 'NONE', #19744, 2.000000000000000000 ) ;
#5563 = DIRECTION ( 'NONE',  ( 0.000000000000000000, 0.000000000000000000, 1.000000000000000000 ) ) ;
#5564 = CARTESIAN_POINT ( 'NONE',  ( 3.890962118697714531E-15, 15.50000000000000000, -40.80000000000000426 ) ) ;
#5565 = VERTEX_POINT ( 'NONE', #21286 ) ;
#5566 = EDGE_CURVE ( 'NONE', #5066, #8782, #8464, .T. ) ;
#5567 = DIRECTION ( 'NONE',  ( 1.000000000000000000, 0.000000000000000000, 0.000000000000000000 ) ) ;
#5568 = ORIENTED_EDGE ( 'NONE', *, *, #12758, .T. ) ;
#5569 = VECTOR ( 'NONE', #4719, 1000.000000000000000 ) ;
#5570 = EDGE_CURVE ( 'NONE', #13580, #13312, #22412, .T. ) ;
#5571 = AXIS2_PLACEMENT_3D ( 'NONE', #21843, #8896, #19897 ) ;
#5572 = EDGE_CURVE ( 'NONE', #4271, #2673, #2853, .T. ) ;
#5573 = ORIENTED_EDGE ( 'NONE', *, *, #3973, .F. ) ;
#5574 = DIRECTION ( 'NONE',  ( 0.000000000000000000, -1.000000000000000000, 0.000000000000000000 ) ) ;
#5575 = VECTOR ( 'NONE', #4072, 1000.000000000000114 ) ;
#5576 = DIRECTION ( 'NONE',  ( -1.000000000000000000, 0.000000000000000000, 0.000000000000000000 ) ) ;
#5577 = DIRECTION ( 'NONE',  ( -1.000000000000000000, 0.000000000000000000, 0.000000000000000000 ) ) ;
#5578 = VECTOR ( 'NONE', #9213, 1000.000000000000000 ) ;
#5579 = AXIS2_PLACEMENT_3D ( 'NONE', #13777, #483, #367 ) ;
#5580 = DIRECTION ( 'NONE',  ( -1.000000000000000000, 0.000000000000000000, 0.000000000000000000 ) ) ;
#5581 = DIRECTION ( 'NONE',  ( -1.000000000000000000, 0.000000000000000000, 0.000000000000000000 ) ) ;
#5582 = CONICAL_SURFACE ( 'NONE', #924, 5.000000000000007994, 0.9599310885968855844 ) ;
#5583 = DIRECTION ( 'NONE',  ( 0.000000000000000000, 0.000000000000000000, 1.000000000000000000 ) ) ;
#5584 = VERTEX_POINT ( 'NONE', #8193 ) ;
#5585 = EDGE_LOOP ( 'NONE', ( #12365, #16918, #23028, #19820, #10427, #22514, #616, #1343, #14933 ) ) ;
#5586 =( REPRESENTATION_RELATIONSHIP ('NONE','NONE', #21748, #19247 ) REPRESENTATION_RELATIONSHIP_WITH_TRANSFORMATION ( #11481 )SHAPE_REPRESENTATION_RELATIONSHIP( ) );
#5587 = CARTESIAN_POINT ( 'NONE',  ( 7.685661446562381371, -5.583959896777971110, 11.00674201446023304 ) ) ;
#5588 = ORIENTED_EDGE ( 'NONE', *, *, #21931, .T. ) ;
#5589 = ORIENTED_EDGE ( 'NONE', *, *, #3914, .F. ) ;
#5590 = CARTESIAN_POINT ( 'NONE',  ( 41.73082370883260239, 29.49999999999999645, -1.500000000000000000 ) ) ;
#5591 = ORIENTED_EDGE ( 'NONE', *, *, #4970, .T. ) ;
#5592 = AXIS2_PLACEMENT_3D ( 'NONE', #4382, #19271, #2554 ) ;
#5593 = DIRECTION ( 'NONE',  ( 1.000000000000000000, 0.000000000000000000, -0.000000000000000000 ) ) ;
#5594 = DIRECTION ( 'NONE',  ( -1.000000000000000000, -0.000000000000000000, -0.000000000000000000 ) ) ;
#5595 = AXIS2_PLACEMENT_3D ( 'NONE', #11727, #3834, #20921 ) ;
#5596 = AXIS2_PLACEMENT_3D ( 'NONE', #13472, #13704, #6399 ) ;
#5597 = ADVANCED_FACE ( 'NONE', ( #17484 ), #12985, .F. ) ;
#5598 = CIRCLE ( 'NONE', #19240, 20.85000000000000853 ) ;
#5599 = VECTOR ( 'NONE', #9773, 1000.000000000000114 ) ;
#5600 = CARTESIAN_POINT ( 'NONE',  ( 23.00000000000000000, -9.239931321968100519, -10.79948145182508057 ) ) ;
#5601 =( LENGTH_UNIT ( ) NAMED_UNIT ( * ) SI_UNIT ( .MILLI., .METRE. ) );
#5602 = FACE_OUTER_BOUND ( 'NONE', #1101, .T. ) ;
#5603 = CIRCLE ( 'NONE', #17276, 5.000000000000004441 ) ;
#5604 = VECTOR ( 'NONE', #3035, 1000.000000000000000 ) ;
#5605 = ADVANCED_FACE ( 'NONE', ( #23371 ), #20396, .T. ) ;
#5606 = EDGE_CURVE ( 'NONE', #22118, #23775, #12582, .T. ) ;
#5607 = CARTESIAN_POINT ( 'NONE',  ( 87.67068093254673045, -5.000000000000000000, 6.123233995736775157E-16 ) ) ;
#5608 = EDGE_CURVE ( 'NONE', #666, #19209, #20923, .T. ) ;
#5609 = CARTESIAN_POINT ( 'NONE',  ( 64.69295543108962931, 7.420530141404717394E-15, 0.000000000000000000 ) ) ;
#5610 = CARTESIAN_POINT ( 'NONE',  ( 80.39795365981946418, -5.000000000000000888, 6.123233995736776143E-16 ) ) ;
#5611 = CARTESIAN_POINT ( 'NONE',  ( -17.59008829125738060, 9.499485695642613692, -0.4958780962348213750 ) ) ;
#5612 = FACE_OUTER_BOUND ( 'NONE', #3048, .T. ) ;
#5613 = DIRECTION ( 'NONE',  ( -1.000000000000000000, -1.224606353822377258E-16, -0.000000000000000000 ) ) ;
#5614 = AXIS2_PLACEMENT_3D ( 'NONE', #17569, #15989, #1126 ) ;
#5615 = FACE_OUTER_BOUND ( 'NONE', #10528, .T. ) ;
#5616 = VERTEX_POINT ( 'NONE', #19084 ) ;
#5617 = DIRECTION ( 'NONE',  ( -0.000000000000000000, -0.000000000000000000, -1.000000000000000000 ) ) ;
#5618 = AXIS2_PLACEMENT_3D ( 'NONE', #12563, #7079, #9020 ) ;
#5619 = ORIENTED_EDGE ( 'NONE', *, *, #15232, .F. ) ;
#5620 = CARTESIAN_POINT ( 'NONE',  ( -41.49999999999999289, -27.79189783386527779, -27.00000000000000000 ) ) ;
#5621 = AXIS2_PLACEMENT_3D ( 'NONE', #13592, #17602, #2855 ) ;
#5622 = AXIS2_PLACEMENT_3D ( 'NONE', #10135, #19560, #11855 ) ;
#5623 = ORIENTED_EDGE ( 'NONE', *, *, #23588, .T. ) ;
#5624 = DIRECTION ( 'NONE',  ( -1.000000000000000000, -1.224606353822377258E-16, -0.000000000000000000 ) ) ;
#5625 = FACE_OUTER_BOUND ( 'NONE', #3819, .T. ) ;
#5626 = DIRECTION ( 'NONE',  ( -1.000000000000000000, -0.000000000000000000, -0.000000000000000000 ) ) ;
#5627 = CONICAL_SURFACE ( 'NONE', #18104, 2.024999999999999911, 0.7853981633974222998 ) ;
#5628 = DIRECTION ( 'NONE',  ( 0.000000000000000000, -1.000000000000000000, 0.000000000000000000 ) ) ;
#5629 = EDGE_CURVE ( 'NONE', #5195, #9278, #2357, .T. ) ;
#5630 = CARTESIAN_POINT ( 'NONE',  ( 65.85249911436491743, -5.000000000000000888, 6.123233995736776143E-16 ) ) ;
#5631 = AXIS2_PLACEMENT_3D ( 'NONE', #8897, #22212, #1590 ) ;
#5632 = CARTESIAN_POINT ( 'NONE',  ( -7.685661446562381371, 5.583959896777970222, -6.859589141758143604 ) ) ;
#5633 = VERTEX_POINT ( 'NONE', #17238 ) ;
#5634 = AXIS2_PLACEMENT_3D ( 'NONE', #18608, #2245, #20562 ) ;
#5635 = ORIENTED_EDGE ( 'NONE', *, *, #9942, .F. ) ;
#5636 = CARTESIAN_POINT ( 'NONE',  ( -43.49999999999997868, -25.84341543330624091, 0.000000000000000000 ) ) ;
#5637 = CARTESIAN_POINT ( 'NONE',  ( -9.000000000000000000, 0.000000000000000000, 0.9999999999999731326 ) ) ;
#5638 = EDGE_CURVE ( 'NONE', #16665, #15653, #1703, .T. ) ;
#5639 = ORIENTED_EDGE ( 'NONE', *, *, #17052, .F. ) ;
#5640 = CARTESIAN_POINT ( 'NONE',  ( 0.000000000000000000, 15.03999999999999915, -27.00000000000000000 ) ) ;
#5641 = AXIS2_PLACEMENT_3D ( 'NONE', #11209, #18681, #4630 ) ;
#5642 = AXIS2_PLACEMENT_3D ( 'NONE', #835, #6815, #12293 ) ;
#5643 = ORIENTED_EDGE ( 'NONE', *, *, #5472, .T. ) ;
#5644 = DIRECTION ( 'NONE',  ( 0.000000000000000000, 0.000000000000000000, -1.000000000000000000 ) ) ;
#5645 = LINE ( 'NONE', #20535, #22376 ) ;
#5646 = VECTOR ( 'NONE', #3378, 1000.000000000000000 ) ;
#5647 = DIRECTION ( 'NONE',  ( 0.000000000000000000, -1.000000000000000000, 0.000000000000000000 ) ) ;
#5648 = EDGE_LOOP ( 'NONE', ( #23254, #10439, #6100, #451, #2234 ) ) ;
#5649 = LINE ( 'NONE', #18811, #7788 ) ;
#5650 = CARTESIAN_POINT ( 'NONE',  ( 71.96568270381689558, 5.000000000000025757, 6.123233995736788962E-16 ) ) ;
#5651 = AXIS2_PLACEMENT_3D ( 'NONE', #1916, #2024, #20589 ) ;
#5652 = VECTOR ( 'NONE', #15907, 1000.000000000000000 ) ;
#5653 = DIRECTION ( 'NONE',  ( -0.000000000000000000, 0.000000000000000000, 1.000000000000000000 ) ) ;
#5654 = ORIENTED_EDGE ( 'NONE', *, *, #19047, .F. ) ;
#5655 = ORIENTED_EDGE ( 'NONE', *, *, #22961, .T. ) ;
#5656 = CIRCLE ( 'NONE', #7559, 1.000000000000000888 ) ;
#5657 = EDGE_LOOP ( 'NONE', ( #15926, #13650, #23544, #18913 ) ) ;
#5658 = VECTOR ( 'NONE', #2415, 1000.000000000000000 ) ;
#5659 = B_SPLINE_CURVE_WITH_KNOTS ( 'NONE', 3,
 ( #14235, #23297, #15836, #8508, #14347, #6927, #8383, #6686, #8861, #14117, #21807, #23411, #12148, #2905, #21336, #3255, #1199, #6809, #19863, #4625, #10454, #19500, #15948, #21577, #10684, #19627, #18155, #12025, #4871, #12404, #17653, #6450 ),
 .UNSPECIFIED., .F., .F.,
 ( 4, 2, 2, 2, 2, 2, 2, 2, 2, 2, 2, 2, 2, 2, 2, 4 ),
 ( 0.000000000000000000, 0.0005902259033179341197, 0.001180451806635868239, 0.001770677709953802359, 0.002360903613271736479, 0.003541355419907607320, 0.004131581323225543174, 0.004721807226543479029, 0.005312033129861415751, 0.005902259033179352472, 0.006492484936497288327, 0.007082710839815223314, 0.007672936743133159168, 0.008263162646451095023, 0.008853388549769029142, 0.009443614453086964997 ),
 .UNSPECIFIED. ) ;
#5660 = ITEM_DEFINED_TRANSFORMATION ( 'NONE', 'NONE', #8023,  #8005 ) ;
#5661 = EDGE_CURVE ( 'NONE', #4711, #20735, #21033, .T. ) ;
#5662 = ORIENTED_EDGE ( 'NONE', *, *, #3792, .F. ) ;
#5663 = CARTESIAN_POINT ( 'NONE',  ( 34.10000000000001563, -29.50000000000000711, 27.00000000000000000 ) ) ;
#5664 = AXIS2_PLACEMENT_3D ( 'NONE', #12551, #16344, #16112 ) ;
#5665 = CIRCLE ( 'NONE', #19306, 6.050000000006051870 ) ;
#5666 = CARTESIAN_POINT ( 'NONE',  ( -41.99999999999999289, 1.286185300804507526E-15, -10.50249999999999950 ) ) ;
#5667 = EDGE_LOOP ( 'NONE', ( #2241, #920, #21764, #13015, #8014 ) ) ;
#5668 = EDGE_CURVE ( 'NONE', #21092, #16520, #21187, .T. ) ;
#5669 = EDGE_CURVE ( 'NONE', #16889, #20379, #23909, .T. ) ;
#5670 = CARTESIAN_POINT ( 'NONE',  ( 20.99999999999999645, 29.50000000000000355, 11.50000000000000000 ) ) ;
#5671 = VERTEX_POINT ( 'NONE', #6886 ) ;
#5672 = CARTESIAN_POINT ( 'NONE',  ( 41.50000000000000000, -27.79189783386526358, -27.00000000000000000 ) ) ;
#5673 = DIRECTION ( 'NONE',  ( 1.000000000000000000, 1.224606353822377258E-16, 0.000000000000000000 ) ) ;
#5674 = CARTESIAN_POINT ( 'NONE',  ( -5.622572944242077574E-13, 8.680847955711007202, -3.133165578109187610 ) ) ;
#5675 = DIRECTION ( 'NONE',  ( -1.000000000000000000, -0.000000000000000000, -0.000000000000000000 ) ) ;
#5676 = CIRCLE ( 'NONE', #21658, 17.25000000000000000 ) ;
#5677 = CARTESIAN_POINT ( 'NONE',  ( 5.000000000000000000, 4.685197434473818312, -1.301042606982605321E-15 ) ) ;
#5678 = ORIENTED_EDGE ( 'NONE', *, *, #2126, .T. ) ;
#5679 = DIRECTION ( 'NONE',  ( 0.000000000000000000, -1.000000000000000000, 0.000000000000000000 ) ) ;
#5680 = DIRECTION ( 'NONE',  ( -0.000000000000000000, -0.000000000000000000, -1.000000000000000000 ) ) ;
#5681 = LINE ( 'NONE', #11249, #16223 ) ;
#5682 = CIRCLE ( 'NONE', #17354, 10.49999999999999822 ) ;
#5683 = AXIS2_PLACEMENT_3D ( 'NONE', #6760, #14190, #16501 ) ;
#5684 = ORIENTED_EDGE ( 'NONE', *, *, #15911, .T. ) ;
#5685 = CARTESIAN_POINT ( 'NONE',  ( -6.233975306307046963E-13, 9.127583699786111282, 7.133165578109187166 ) ) ;
#5686 = VERTEX_POINT ( 'NONE', #4946 ) ;
#5687 = ADVANCED_FACE ( 'NONE', ( #1156 ), #19241, .T. ) ;
#5688 = APPLICATION_PROTOCOL_DEFINITION ( 'draft international standard', 'automotive_design', 1998, #21484 ) ;
#5689 = EDGE_LOOP ( 'NONE', ( #6694, #15031, #19094, #1460 ) ) ;
#5690 = ORIENTED_EDGE ( 'NONE', *, *, #762, .F. ) ;
#5691 = EDGE_CURVE ( 'NONE', #14561, #5160, #23607, .T. ) ;
#5692 = DIRECTION ( 'NONE',  ( -1.000000000000000000, -1.224606353822377258E-16, -0.000000000000000000 ) ) ;
#5693 = CARTESIAN_POINT ( 'NONE',  ( -8.680847955711200825, 2.820578480813073607, -9.533165578109187521 ) ) ;
#5694 = AXIS2_PLACEMENT_3D ( 'NONE', #4929, #12570, #16251 ) ;
#5695 = AXIS2_PLACEMENT_3D ( 'NONE', #19520, #14373, #1223 ) ;
#5696 = CARTESIAN_POINT ( 'NONE',  ( 0.000000000000000000, 0.000000000000000000, 0.9999999999999731326 ) ) ;
#5697 = EDGE_CURVE ( 'NONE', #16388, #18576, #12717, .T. ) ;
#5698 = AXIS2_PLACEMENT_3D ( 'NONE', #16092, #10478, #3162 ) ;
#5699 = ORIENTED_EDGE ( 'NONE', *, *, #20810, .F. ) ;
#5700 = CARTESIAN_POINT ( 'NONE',  ( 1.999999999999994449, -45.00000000000000000, -23.99999999999999645 ) ) ;
#5701 = CYLINDRICAL_SURFACE ( 'NONE', #17784, 1.000000000000000000 ) ;
#5702 = FACE_BOUND ( 'NONE', #8465, .T. ) ;
#5703 = PRODUCT ( 'Pin 2X4', 'Pin 2X4', '', ( #18854 ) ) ;
#5704 = AXIS2_PLACEMENT_3D ( 'NONE', #12427, #19888, #6596 ) ;
#5705 = DIRECTION ( 'NONE',  ( 0.000000000000000000, -1.000000000000000000, 0.000000000000000000 ) ) ;
#5706 = VERTEX_POINT ( 'NONE', #20056 ) ;
#5707 = CIRCLE ( 'NONE', #22462, 2.024999999999999911 ) ;
#5708 = DIRECTION ( 'NONE',  ( 0.000000000000000000, 1.000000000000000000, -0.000000000000000000 ) ) ;
#5709 = ORIENTED_EDGE ( 'NONE', *, *, #8040, .T. ) ;
#5710 = ORIENTED_EDGE ( 'NONE', *, *, #5164, .T. ) ;
#5711 = CARTESIAN_POINT ( 'NONE',  ( -9.500000000000000000, -6.482511860946779655E-13, -7.059589141758143782 ) ) ;
#5712 = CARTESIAN_POINT ( 'NONE',  ( 33.99999999999998579, 3.999999999999985345, 9.500000000000000000 ) ) ;
#5713 = FACE_OUTER_BOUND ( 'NONE', #353, .T. ) ;
#5714 = FACE_OUTER_BOUND ( 'NONE', #21852, .T. ) ;
#5715 = CARTESIAN_POINT ( 'NONE',  ( -7.999999999999986677, 0.000000000000000000, 53.00000000000000000 ) ) ;
#5716 = PRODUCT_DEFINITION_FORMATION_WITH_SPECIFIED_SOURCE ( 'ANY', '', #16053, .NOT_KNOWN. ) ;
#5717 = VERTEX_POINT ( 'NONE', #20177 ) ;
#5718 = AXIS2_PLACEMENT_3D ( 'NONE', #15658, #6414, #13859 ) ;
#5719 = ORIENTED_EDGE ( 'NONE', *, *, #19028, .F. ) ;
#5720 = VERTEX_POINT ( 'NONE', #17867 ) ;
#5721 = ORIENTED_EDGE ( 'NONE', *, *, #21560, .F. ) ;
#5722 = AXIS2_PLACEMENT_3D ( 'NONE', #10609, #18083, #20157 ) ;
#5723 = EDGE_CURVE ( 'NONE', #2790, #11994, #4836, .T. ) ;
#5724 = CARTESIAN_POINT ( 'NONE',  ( -31.74999999999995737, 6.123233995736767268E-16, -5.000000000000000888 ) ) ;
#5725 = ADVANCED_FACE ( 'NONE', ( #16015 ), #23719, .T. ) ;
#5726 = CARTESIAN_POINT ( 'NONE',  ( 7.937578510445358226, -3.514536757623690999, 12.49999999999999112 ) ) ;
#5727 = DIRECTION ( 'NONE',  ( 0.000000000000000000, 0.000000000000000000, 1.000000000000000000 ) ) ;
#5728 = CARTESIAN_POINT ( 'NONE',  ( -28.27483331787890819, -41.23752903419608629, 27.00000000000000000 ) ) ;
#5729 = AXIS2_PLACEMENT_3D ( 'NONE', #2710, #19180, #13813 ) ;
#5730 = CARTESIAN_POINT ( 'NONE',  ( 21.13207267780287069, -38.32709852940855910, 0.000000000000000000 ) ) ;
#5731 = ORIENTED_EDGE ( 'NONE', *, *, #18298, .F. ) ;
#5732 = CARTESIAN_POINT ( 'NONE',  ( 23.84999999999999432, -15.03999999999999559, -25.00000000000000000 ) ) ;
#5733 = DIRECTION ( 'NONE',  ( -1.000000000000000000, 0.000000000000000000, 0.000000000000000000 ) ) ;
#5734 = DIRECTION ( 'NONE',  ( 0.000000000000000000, 0.000000000000000000, 1.000000000000000000 ) ) ;
#5735 = CARTESIAN_POINT ( 'NONE',  ( -17.15849686392983031, 8.309918483244986831, 4.628645577532792821 ) ) ;
#5736 = APPLICATION_CONTEXT ( 'automotive_design' ) ;
#5737 = DIRECTION ( 'NONE',  ( -0.000000000000000000, 1.000000000000000000, 1.224646799147353207E-16 ) ) ;
#5738 = ORIENTED_EDGE ( 'NONE', *, *, #23440, .F. ) ;
#5739 = PRODUCT_RELATED_PRODUCT_CATEGORY ( 'part', '', ( #19570 ) ) ;
#5740 = DIRECTION ( 'NONE',  ( -1.000000000000000000, 0.000000000000000000, -0.000000000000000000 ) ) ;
#5741 = EDGE_LOOP ( 'NONE', ( #13060, #20160, #12352, #12019, #20057 ) ) ;
#5742 = ADVANCED_FACE ( 'NONE', ( #8689 ), #4029, .F. ) ;
#5743 = FACE_OUTER_BOUND ( 'NONE', #21744, .T. ) ;
#5744 = ORIENTED_EDGE ( 'NONE', *, *, #17301, .F. ) ;
#5745 = CARTESIAN_POINT ( 'NONE',  ( -31.74999999999995737, 0.000000000000000000, 0.000000000000000000 ) ) ;
#5746 = VERTEX_POINT ( 'NONE', #10634 ) ;
#5747 = ADVANCED_FACE ( 'NONE', ( #19823 ), #15311, .T. ) ;
#5748 = DIRECTION ( 'NONE',  ( 0.000000000000000000, 0.000000000000000000, 1.000000000000000000 ) ) ;
#5749 = CARTESIAN_POINT ( 'NONE',  ( 10.40000000000000036, 0.000000000000000000, 0.000000000000000000 ) ) ;
#5750 = CYLINDRICAL_SURFACE ( 'NONE', #6095, 5.000000000000000888 ) ;
#5751 = EDGE_CURVE ( 'NONE', #6020, #14543, #8704, .T. ) ;
#5752 = DIRECTION ( 'NONE',  ( -0.000000000000000000, -0.000000000000000000, 1.000000000000000000 ) ) ;
#5753 = EDGE_CURVE ( 'NONE', #17625, #6136, #6987, .T. ) ;
#5754 = FACE_OUTER_BOUND ( 'NONE', #13457, .T. ) ;
#5755 = CARTESIAN_POINT ( 'NONE',  ( -9.500000000000000000, -6.482511860946779655E-13, -9.059589141758143782 ) ) ;
#5756 = ORIENTED_EDGE ( 'NONE', *, *, #15832, .F. ) ;
#5757 = DIRECTION ( 'NONE',  ( -1.000000000000000000, 0.000000000000000000, 0.000000000000000000 ) ) ;
#5758 = CARTESIAN_POINT ( 'NONE',  ( 3.000000000000000888, 6.000000000000000000, 80.99999999999998579 ) ) ;
#5759 = ORIENTED_EDGE ( 'NONE', *, *, #5606, .T. ) ;
#5760 = CARTESIAN_POINT ( 'NONE',  ( 35.99999999999999289, 50.99999999999999289, 0.5000000000000000000 ) ) ;
#5761 = CARTESIAN_POINT ( 'NONE',  ( 0.000000000000000000, -45.00000000000000000, -27.00000000000000000 ) ) ;
#5762 = CARTESIAN_POINT ( 'NONE',  ( 14.94708199919714531, 1.300481340138145203, -9.416259293296516120 ) ) ;
#5763 = CARTESIAN_POINT ( 'NONE',  ( -3.000000000000000444, 8.485281374238569541, 80.80041615069272609 ) ) ;
#5764 = CARTESIAN_POINT ( 'NONE',  ( 0.000000000000000000, 32.75000000000000000, 14.70000000000000284 ) ) ;
#5765 = CARTESIAN_POINT ( 'NONE',  ( 29.00000000000000355, 29.50000000000000000, 27.00000000000000000 ) ) ;
#5766 = ADVANCED_FACE ( 'NONE', ( #16263 ), #21768, .T. ) ;
#5767 = DIRECTION ( 'NONE',  ( -1.000000000000000000, 0.000000000000000000, 0.000000000000000000 ) ) ;
#5768 = ORIENTED_EDGE ( 'NONE', *, *, #14299, .T. ) ;
#5769 = DIRECTION ( 'NONE',  ( -0.000000000000000000, -0.000000000000000000, -1.000000000000000000 ) ) ;
#5770 = CARTESIAN_POINT ( 'NONE',  ( 0.000000000000000000, 15.03999999999999737, 2.200000000000000178 ) ) ;
#5771 = CARTESIAN_POINT ( 'NONE',  ( 40.29291594121673370, 26.62062637246459218, 11.00000000000000000 ) ) ;
#5772 = CYLINDRICAL_SURFACE ( 'NONE', #23489, 18.50000000000000000 ) ;
#5773 = EDGE_LOOP ( 'NONE', ( #19559, #1851, #2866, #13206, #6319 ) ) ;
#5774 = EDGE_CURVE ( 'NONE', #2874, #10068, #3247, .T. ) ;
#5775 = ADVANCED_FACE ( 'NONE', ( #10866 ), #19637, .T. ) ;
#5776 = VERTEX_POINT ( 'NONE', #3335 ) ;
#5777 = ITEM_DEFINED_TRANSFORMATION ( 'NONE', 'NONE', #9590,  #2965 ) ;
#5778 = VERTEX_POINT ( 'NONE', #10758 ) ;
#5779 = DIRECTION ( 'NONE',  ( -0.000000000000000000, -0.000000000000000000, -1.000000000000000000 ) ) ;
#5780 = CARTESIAN_POINT ( 'NONE',  ( -28.00000000000001066, 50.99999999999999289, 0.000000000000000000 ) ) ;
#5781 = CARTESIAN_POINT ( 'NONE',  ( 9.500000000000000000, 6.470877716354879437E-13, 9.206742014460234103 ) ) ;
#5782 = ORIENTED_EDGE ( 'NONE', *, *, #19600, .T. ) ;
#5783 = VERTEX_POINT ( 'NONE', #10517 ) ;
#5784 = CARTESIAN_POINT ( 'NONE',  ( 85.05659179472598908, -5.000000000000009770, 0.000000000000000000 ) ) ;
#5785 = ORIENTED_EDGE ( 'NONE', *, *, #23042, .T. ) ;
#5786 = CARTESIAN_POINT ( 'NONE',  ( -0.9830802669677241035, 45.00000000000000000, 4.201721238055123209 ) ) ;
#5787 = FACE_OUTER_BOUND ( 'NONE', #23488, .T. ) ;
#5788 = CARTESIAN_POINT ( 'NONE',  ( 0.000000000000000000, 14.21257171757157955, -0.08908218613038007549 ) ) ;
#5789 = CARTESIAN_POINT ( 'NONE',  ( -6.249999999999999112, -10.82531754730548279, 2.500000000000000000 ) ) ;
#5790 = VERTEX_POINT ( 'NONE', #19927 ) ;
#5791 = CARTESIAN_POINT ( 'NONE',  ( 2.570122167802765922, 0.000000000000000000, 0.000000000000000000 ) ) ;
#5792 = CARTESIAN_POINT ( 'NONE',  ( 35.99999999999999289, -51.00000000000000711, 12.50000000000000000 ) ) ;
#5793 = ORIENTED_EDGE ( 'NONE', *, *, #7503, .T. ) ;
#5794 = VERTEX_POINT ( 'NONE', #18107 ) ;
#5795 = CARTESIAN_POINT ( 'NONE',  ( -8.680847955711200825, 2.820578480813073607, 7.533165578109188409 ) ) ;
#5796 = VERTEX_POINT ( 'NONE', #1401 ) ;
#5797 = EDGE_CURVE ( 'NONE', #3463, #16889, #8926, .T. ) ;
#5798 = SHAPE_DEFINITION_REPRESENTATION ( #5156, #23741 ) ;
#5799 = VERTEX_POINT ( 'NONE', #286 ) ;
#5800 = ORIENTED_EDGE ( 'NONE', *, *, #14707, .T. ) ;
#5801 = DIRECTION ( 'NONE',  ( 0.000000000000000000, 1.000000000000000000, 0.000000000000000000 ) ) ;
#5802 = CARTESIAN_POINT ( 'NONE',  ( -7.685661446562381371, 5.583959896777970222, -2.859589141758144493 ) ) ;
#5803 = CARTESIAN_POINT ( 'NONE',  ( 2.570122167802765922, 0.000000000000000000, 0.000000000000000000 ) ) ;
#5804 = ORIENTED_EDGE ( 'NONE', *, *, #5367, .T. ) ;
#5805 = FACE_OUTER_BOUND ( 'NONE', #8558, .T. ) ;
#5806 = LINE ( 'NONE', #2014, #18171 ) ;
#5807 = CARTESIAN_POINT ( 'NONE',  ( -41.49999999999999289, 27.79189783386526358, 27.00000000000000000 ) ) ;
#5808 = CYLINDRICAL_SURFACE ( 'NONE', #12245, 5.000000000000000888 ) ;
#5809 = DIRECTION ( 'NONE',  ( 0.000000000000000000, 0.000000000000000000, 1.000000000000000000 ) ) ;
#5810 = EDGE_LOOP ( 'NONE', ( #22785, #11840 ) ) ;
#5811 = DIRECTION ( 'NONE',  ( -1.000000000000000000, 0.000000000000000000, 0.000000000000000000 ) ) ;
#5812 = EDGE_CURVE ( 'NONE', #4938, #21420, #21585, .T. ) ;
#5813 = DIRECTION ( 'NONE',  ( 0.000000000000000000, -1.000000000000000000, 0.000000000000000000 ) ) ;
#5814 =( NAMED_UNIT ( * ) PLANE_ANGLE_UNIT ( ) SI_UNIT ( $, .RADIAN. ) );
#5815 = DIRECTION ( 'NONE',  ( -0.7089874389501527041, 0.7052211081716879271, 0.000000000000000000 ) ) ;
#5816 = CARTESIAN_POINT ( 'NONE',  ( -23.85000000000000142, 15.03999999999999737, 0.000000000000000000 ) ) ;
#5817 = CARTESIAN_POINT ( 'NONE',  ( 6.809999908187194197E-13, -9.988891130263535700, -5.559589141758142894 ) ) ;
#5818 = EDGE_CURVE ( 'NONE', #11492, #20529, #14928, .T. ) ;
#5819 = CARTESIAN_POINT ( 'NONE',  ( -5.365059087799948223, 7.384370330706355290, -11.33316557810918646 ) ) ;
#5820 =( NAMED_UNIT ( * ) SI_UNIT ( $, .STERADIAN. ) SOLID_ANGLE_UNIT ( ) );
#5821 = VERTEX_POINT ( 'NONE', #13070 ) ;
#5822 = ADVANCED_FACE ( 'NONE', ( #12945 ), #20285, .F. ) ;
#5823 = ORIENTED_EDGE ( 'NONE', *, *, #9801, .F. ) ;
#5824 = EDGE_CURVE ( 'NONE', #15940, #47, #7566, .T. ) ;
#5825 = CIRCLE ( 'NONE', #19474, 1.999999999999994449 ) ;
#5826 = VERTEX_POINT ( 'NONE', #16972 ) ;
#5827 = VERTEX_POINT ( 'NONE', #24061 ) ;
#5828 = ORIENTED_EDGE ( 'NONE', *, *, #17877, .F. ) ;
#5829 = DIRECTION ( 'NONE',  ( 0.000000000000000000, 0.000000000000000000, 1.000000000000000000 ) ) ;
#5830 = DIRECTION ( 'NONE',  ( -1.000000000000000000, 0.000000000000000000, 0.000000000000000000 ) ) ;
#5831 = VECTOR ( 'NONE', #19493, 1000.000000000000000 ) ;
#5832 = CIRCLE ( 'NONE', #22587, 18.49999999999999645 ) ;
#5833 = DIRECTION ( 'NONE',  ( -1.000000000000000000, 0.000000000000000000, 0.000000000000000000 ) ) ;
#5834 = CARTESIAN_POINT ( 'NONE',  ( 10.83999999999999986, -14.99147757894464306, 15.50000000000000000 ) ) ;
#5835 = DIRECTION ( 'NONE',  ( 0.000000000000000000, -1.000000000000000000, 0.000000000000000000 ) ) ;
#5836 = CARTESIAN_POINT ( 'NONE',  ( -5.871322893124554021, 8.081182679343978492, -5.906742014460232504 ) ) ;
#5837 = DIRECTION ( 'NONE',  ( -0.000000000000000000, -0.000000000000000000, -1.000000000000000000 ) ) ;
#5838 = ORIENTED_EDGE ( 'NONE', *, *, #5818, .F. ) ;
#5839 = DIRECTION ( 'NONE',  ( -1.000000000000000000, 0.000000000000000000, 0.000000000000000000 ) ) ;
#5840 = EDGE_CURVE ( 'NONE', #13339, #21886, #11811, .T. ) ;
#5841 = DIRECTION ( 'NONE',  ( 0.000000000000000000, 1.000000000000000000, 0.000000000000000000 ) ) ;
#5842 = DIRECTION ( 'NONE',  ( 0.5735764363510424957, 0.8191520442889943521, 0.000000000000000000 ) ) ;
#5843 = CARTESIAN_POINT ( 'NONE',  ( 68.76159002345582394, -1.078520768856852078E-29, 5.000000000000007994 ) ) ;
#5844 = DIRECTION ( 'NONE',  ( 1.000000000000000000, 0.000000000000000000, -0.000000000000000000 ) ) ;
#5845 = EDGE_CURVE ( 'NONE', #10567, #20508, #1328, .T. ) ;
#5846 = VERTEX_POINT ( 'NONE', #9382 ) ;
#5847 = EDGE_CURVE ( 'NONE', #8138, #12085, #17663, .T. ) ;
#5848 = CARTESIAN_POINT ( 'NONE',  ( -23.85000000000000142, -15.03999999999999737, 2.200000000000000178 ) ) ;
#5849 = ORIENTED_EDGE ( 'NONE', *, *, #17199, .F. ) ;
#5850 = CARTESIAN_POINT ( 'NONE',  ( 0.000000000000000000, -15.03999999999999915, -25.00000000000000000 ) ) ;
#5851 = VERTEX_POINT ( 'NONE', #1862 ) ;
#5852 = CARTESIAN_POINT ( 'NONE',  ( -5.871322893123450015, -8.081182679344781405, 9.359589141758146269 ) ) ;
#5853 = ORIENTED_EDGE ( 'NONE', *, *, #8242, .F. ) ;
#5854 = DIRECTION ( 'NONE',  ( -0.5735764363510519326, 0.8191520442889876907, 1.003171929053519816E-16 ) ) ;
#5855 = DIRECTION ( 'NONE',  ( 0.000000000000000000, 0.000000000000000000, 1.000000000000000000 ) ) ;
#5856 = FACE_OUTER_BOUND ( 'NONE', #9886, .T. ) ;
#5857 = PLANE ( 'NONE',  #23228 ) ;
#5858 = CARTESIAN_POINT ( 'NONE',  ( 35.99999999999999289, 50.99999999999999289, 12.50000000000000000 ) ) ;
#5859 = CARTESIAN_POINT ( 'NONE',  ( 5.871322893124553133, -8.081182679343980269, -9.759589141758143072 ) ) ;
#5860 = EDGE_LOOP ( 'NONE', ( #11123, #6742, #23832, #2602 ) ) ;
#5861 = CONICAL_SURFACE ( 'NONE', #2344, 2.024999999999999911, 0.7853981633974743692 ) ;
#5862 = CARTESIAN_POINT ( 'NONE',  ( 7.685661446561619314, 5.583959896779020049, 11.40674201446023517 ) ) ;
#5863 = ORIENTED_EDGE ( 'NONE', *, *, #15730, .T. ) ;
#5864 = CARTESIAN_POINT ( 'NONE',  ( 71.67068093254673045, -5.000000000000000000, 6.123233995736775157E-16 ) ) ;
#5865 = DIRECTION ( 'NONE',  ( -0.000000000000000000, -1.000000000000000000, -0.000000000000000000 ) ) ;
#5866 = FACE_BOUND ( 'NONE', #11406, .T. ) ;
#5867 = CARTESIAN_POINT ( 'NONE',  ( 0.000000000000000000, 0.000000000000000000, 15.50000000000000000 ) ) ;
#5868 = EDGE_CURVE ( 'NONE', #2103, #15317, #23534, .T. ) ;
#5869 = DIRECTION ( 'NONE',  ( 0.000000000000000000, 0.000000000000000000, 1.000000000000000000 ) ) ;
#5870 = EDGE_CURVE ( 'NONE', #14363, #19452, #141, .T. ) ;
#5871 = DIRECTION ( 'NONE',  ( 0.000000000000000000, 1.000000000000000000, 0.000000000000000000 ) ) ;
#5872 = DIRECTION ( 'NONE',  ( 0.000000000000000000, 0.000000000000000000, -1.000000000000000000 ) ) ;
#5873 = ORIENTED_EDGE ( 'NONE', *, *, #18435, .T. ) ;
#5874 = DIRECTION ( 'NONE',  ( 0.000000000000000000, -1.000000000000000000, 0.000000000000000000 ) ) ;
#5875 = CARTESIAN_POINT ( 'NONE',  ( 0.000000000000000000, 11.90821470209324140, 7.758837095328885880 ) ) ;
#5876 = DIRECTION ( 'NONE',  ( -1.000000000000000000, 0.000000000000000000, 0.000000000000000000 ) ) ;
#5877 = FACE_OUTER_BOUND ( 'NONE', #3632, .T. ) ;
#5878 = DIRECTION ( 'NONE',  ( 0.000000000000000000, -1.000000000000000000, 0.000000000000000000 ) ) ;
#5879 = AXIS2_PLACEMENT_3D ( 'NONE', #4979, #945, #12389 ) ;
#5880 = ORIENTED_EDGE ( 'NONE', *, *, #9299, .F. ) ;
#5881 = ORIENTED_EDGE ( 'NONE', *, *, #23632, .T. ) ;
#5882 = CIRCLE ( 'NONE', #8217, 11.00000000000000000 ) ;
#5883 = ORIENTED_EDGE ( 'NONE', *, *, #11948, .F. ) ;
#5884 = ORIENTED_EDGE ( 'NONE', *, *, #21760, .T. ) ;
#5885 = FACE_OUTER_BOUND ( 'NONE', #11555, .T. ) ;
#5886 = ADVANCED_FACE ( 'NONE', ( #9282 ), #15012, .T. ) ;
#5887 = CARTESIAN_POINT ( 'NONE',  ( -28.27483331787888687, 41.23752903419610050, 12.00000000000000000 ) ) ;
#5888 = EDGE_LOOP ( 'NONE', ( #11999, #24043, #88, #8112 ) ) ;
#5889 = CARTESIAN_POINT ( 'NONE',  ( -41.99999999999999289, 0.000000000000000000, 0.000000000000000000 ) ) ;
#5890 = FACE_OUTER_BOUND ( 'NONE', #16010, .T. ) ;
#5891 = ORIENTED_EDGE ( 'NONE', *, *, #19464, .T. ) ;
#5892 = AXIS2_PLACEMENT_3D ( 'NONE', #996, #10108, #1118 ) ;
#5893 =( REPRESENTATION_RELATIONSHIP ('NONE','NONE', #2851, #6130 ) REPRESENTATION_RELATIONSHIP_WITH_TRANSFORMATION ( #21389 )SHAPE_REPRESENTATION_RELATIONSHIP( ) );
#5894 = ADVANCED_FACE ( 'NONE', ( #16727 ), #22593, .F. ) ;
#5895 = ORIENTED_EDGE ( 'NONE', *, *, #23362, .T. ) ;
#5896 = EDGE_CURVE ( 'NONE', #15333, #9132, #23126, .T. ) ;
#5897 = DIRECTION ( 'NONE',  ( 1.000000000000000000, 0.000000000000000000, -0.000000000000000000 ) ) ;
#5898 = CARTESIAN_POINT ( 'NONE',  ( 80.69295543108962931, 5.000000000000007105, 6.123233995736765296E-16 ) ) ;
#5899 = VECTOR ( 'NONE', #22391, 1000.000000000000000 ) ;
#5900 = DIRECTION ( 'NONE',  ( -0.000000000000000000, -0.000000000000000000, -1.000000000000000000 ) ) ;
#5901 = LINE ( 'NONE', #18715, #8745 ) ;
#5902 = ORIENTED_EDGE ( 'NONE', *, *, #23672, .F. ) ;
#5903 = DIRECTION ( 'NONE',  ( -1.000000000000000000, 0.000000000000000000, 0.000000000000000000 ) ) ;
#5904 = FACE_OUTER_BOUND ( 'NONE', #16920, .T. ) ;
#5905 = CARTESIAN_POINT ( 'NONE',  ( 29.00000000000000000, -29.50000000000000355, 12.00000000000000000 ) ) ;
#5906 = ORIENTED_EDGE ( 'NONE', *, *, #8251, .F. ) ;
#5907 = EDGE_LOOP ( 'NONE', ( #13914, #16950, #22525, #10405, #4551, #17152 ) ) ;
#5908 = CARTESIAN_POINT ( 'NONE',  ( -5.365059087798939252, -7.384370330707086261, 5.933165578109187877 ) ) ;
#5909 = VERTEX_POINT ( 'NONE', #3809 ) ;
#5910 = DIRECTION ( 'NONE',  ( -1.000000000000000000, -1.224606353822377258E-16, -0.000000000000000000 ) ) ;
#5911 =( GEOMETRIC_REPRESENTATION_CONTEXT ( 3 ) GLOBAL_UNCERTAINTY_ASSIGNED_CONTEXT ( ( #17651 ) ) GLOBAL_UNIT_ASSIGNED_CONTEXT ( ( #22675, #4146, #2303 ) ) REPRESENTATION_CONTEXT ( 'NONE', 'WORKASPACE' ) );
#5912 = VERTEX_POINT ( 'NONE', #2093 ) ;
#5913 = ORIENTED_EDGE ( 'NONE', *, *, #16180, .T. ) ;
#5914 = CARTESIAN_POINT ( 'NONE',  ( 29.00000000000000355, 29.50000000000000000, -27.00000000000000000 ) ) ;
#5915 = CARTESIAN_POINT ( 'NONE',  ( -9.500000000000000000, -6.482511860946779655E-13, -3.059589141758143338 ) ) ;
#5916 = AXIS2_PLACEMENT_3D ( 'NONE', #19081, #2354, #7954 ) ;
#5917 = FACE_OUTER_BOUND ( 'NONE', #4728, .T. ) ;
#5918 = EDGE_CURVE ( 'NONE', #12230, #15766, #13183, .T. ) ;
#5919 = ORIENTED_EDGE ( 'NONE', *, *, #11874, .F. ) ;
#5920 = CARTESIAN_POINT ( 'NONE',  ( -41.00000000000000000, -26.23076770084981746, 12.00000000000000000 ) ) ;
#5921 = DIRECTION ( 'NONE',  ( -1.000000000000000000, 0.000000000000000000, 0.000000000000000000 ) ) ;
#5922 = CYLINDRICAL_SURFACE ( 'NONE', #2840, 9.499999999999987566 ) ;
#5923 = CARTESIAN_POINT ( 'NONE',  ( 0.000000000000000000, 0.000000000000000000, 6.000000000000000000 ) ) ;
#5924 = VERTEX_POINT ( 'NONE', #20642 ) ;
#5926 = EDGE_CURVE ( 'NONE', #12319, #14989, #13298, .T. ) ;
#5925 = CARTESIAN_POINT ( 'NONE',  ( -9.000000000000000000, 0.000000000000000000, 103.9999999999999858 ) ) ;
#5927 = ORIENTED_EDGE ( 'NONE', *, *, #23717, .T. ) ;
#5928 = CARTESIAN_POINT ( 'NONE',  ( -2.935661446561384391, -9.035036904804158553, -7.459589141758144137 ) ) ;
#5929 = EDGE_CURVE ( 'NONE', #13005, #15853, #919, .T. ) ;
#5930 = DIRECTION ( 'NONE',  ( -0.000000000000000000, -0.000000000000000000, -1.000000000000000000 ) ) ;
#5931 = FACE_OUTER_BOUND ( 'NONE', #15192, .T. ) ;
#5932 = CARTESIAN_POINT ( 'NONE',  ( 14.51962751333974389, 3.765689428759031010, -8.721787840009197268 ) ) ;
#5933 = EDGE_CURVE ( 'NONE', #14695, #21357, #18458, .T. ) ;
#5934 = VECTOR ( 'NONE', #18273, 1000.000000000000000 ) ;
#5935 = VECTOR ( 'NONE', #15465, 1000.000000000000000 ) ;
#5936 = DIRECTION ( 'NONE',  ( -1.000000000000000000, 0.000000000000000000, 0.000000000000000000 ) ) ;
#5937 = CARTESIAN_POINT ( 'NONE',  ( -6.233975306307045953E-13, 9.127583699786111282, -11.13316557810918894 ) ) ;
#5938 = VECTOR ( 'NONE', #1969, 999.9999999999998863 ) ;
#5939 = AXIS2_PLACEMENT_3D ( 'NONE', #5097, #19870, #971 ) ;
#5940 = CIRCLE ( 'NONE', #11748, 1.000000000000000888 ) ;
#5941 =( LENGTH_UNIT ( ) NAMED_UNIT ( * ) SI_UNIT ( .MILLI., .METRE. ) );
#5942 = VERTEX_POINT ( 'NONE', #9304 ) ;
#5943 = ORIENTED_EDGE ( 'NONE', *, *, #19026, .T. ) ;
#5944 = CIRCLE ( 'NONE', #9049, 4.057500000000000107 ) ;
#5945 = ORIENTED_EDGE ( 'NONE', *, *, #22102, .F. ) ;
#5946 = FACE_OUTER_BOUND ( 'NONE', #10526, .T. ) ;
#5947 = UNCERTAINTY_MEASURE_WITH_UNIT (LENGTH_MEASURE( 1.000000000000000082E-05 ), #13251, 'distance_accuracy_value', 'NONE');
#5948 = ADVANCED_FACE ( 'NONE', ( #3476 ), #18713, .F. ) ;
#5949 = FACE_OUTER_BOUND ( 'NONE', #17144, .T. ) ;
#5950 = CYLINDRICAL_SURFACE ( 'NONE', #15807, 4.249999999999996447 ) ;
#5951 = CARTESIAN_POINT ( 'NONE',  ( 0.000000000000000000, -1.934484387512043435, 14.08058594723506474 ) ) ;
#5952 = CYLINDRICAL_SURFACE ( 'NONE', #8277, 1.500000000000001332 ) ;
#5953 = EDGE_CURVE ( 'NONE', #16325, #12105, #17001, .T. ) ;
#5954 = VERTEX_POINT ( 'NONE', #15040 ) ;
#5955 = AXIS2_PLACEMENT_3D ( 'NONE', #7781, #22571, #14994 ) ;
#5956 = VECTOR ( 'NONE', #23071, 1000.000000000000000 ) ;
#5957 = AXIS2_PLACEMENT_3D ( 'NONE', #11318, #18796, #2443 ) ;
#5958 = VECTOR ( 'NONE', #23683, 1000.000000000000000 ) ;
#5959 = CIRCLE ( 'NONE', #3221, 9.499999999999994671 ) ;
#5960 = PLANE ( 'NONE',  #98 ) ;
#5961 = VERTEX_POINT ( 'NONE', #3833 ) ;
#5962 = CIRCLE ( 'NONE', #13747, 4.499999999999997335 ) ;
#5963 = EDGE_CURVE ( 'NONE', #145, #13833, #21916, .T. ) ;
#5964 = CARTESIAN_POINT ( 'NONE',  ( 74.57977184163763695, 5.000000000000015099, 0.000000000000000000 ) ) ;
#5965 = EDGE_CURVE ( 'NONE', #17123, #13005, #3208, .T. ) ;
#5966 = DIRECTION ( 'NONE',  ( -0.000000000000000000, -0.000000000000000000, -1.000000000000000000 ) ) ;
#5967 = AXIS2_PLACEMENT_3D ( 'NONE', #11202, #5498, #18677 ) ;
#5968 = LINE ( 'NONE', #13400, #23097 ) ;
#5969 = DIRECTION ( 'NONE',  ( 0.000000000000000000, -1.224646799147353207E-16, 1.000000000000000000 ) ) ;
#5970 = VERTEX_POINT ( 'NONE', #22510 ) ;
#5971 = ORIENTED_EDGE ( 'NONE', *, *, #9291, .T. ) ;
#5972 = ORIENTED_EDGE ( 'NONE', *, *, #18094, .T. ) ;
#5973 = CIRCLE ( 'NONE', #6746, 1.000000000000000888 ) ;
#5974 = CARTESIAN_POINT ( 'NONE',  ( -9.500000000000211386, 3.086737114211961064, 10.95958914175814414 ) ) ;
#5975 = AXIS2_PLACEMENT_3D ( 'NONE', #6818, #9107, #3146 ) ;
#5976 = CONICAL_SURFACE ( 'NONE', #6362, 9.000000000000000000, 0.7853981633974473908 ) ;
#5977 = ORIENTED_EDGE ( 'NONE', *, *, #23194, .T. ) ;
#5978 = CARTESIAN_POINT ( 'NONE',  ( 0.000000000000000000, 0.000000000000000000, 0.000000000000000000 ) ) ;
#5979 = CARTESIAN_POINT ( 'NONE',  ( 1.499999999999999556, 1.836970198721029441E-16, 6.000000000000000000 ) ) ;
#5980 = VECTOR ( 'NONE', #6756, 1000.000000000000000 ) ;
#5981 = DIRECTION ( 'NONE',  ( 0.000000000000000000, 1.000000000000000000, 3.469446951953610639E-15 ) ) ;
#5982 = DIRECTION ( 'NONE',  ( -1.000000000000000000, 2.600433232233976523E-16, -0.000000000000000000 ) ) ;
#5983 = CARTESIAN_POINT ( 'NONE',  ( 4.159489978096820195, -7.970633069177153196, -12.49999999999999822 ) ) ;
#5984 = DIRECTION ( 'NONE',  ( 0.000000000000000000, 0.000000000000000000, 1.000000000000000000 ) ) ;
#5985 = EDGE_CURVE ( 'NONE', #12105, #22724, #5536, .T. ) ;
#5986 = DIRECTION ( 'NONE',  ( 0.000000000000000000, -1.000000000000000000, 0.000000000000000000 ) ) ;
#5987 = ORIENTED_EDGE ( 'NONE', *, *, #9494, .F. ) ;
#5988 = LINE ( 'NONE', #11579, #17212 ) ;
#5989=STYLED_ITEM('',(#24134),#10155);
#5990 = ORIENTED_EDGE ( 'NONE', *, *, #12020, .F. ) ;
#5991 = CARTESIAN_POINT ( 'NONE',  ( -36.00000000000000711, -51.00000000000000711, 0.000000000000000000 ) ) ;
#5992 = CARTESIAN_POINT ( 'NONE',  ( 9.324366632326096311E-16, 9.000000000000000000, 77.99999999999998579 ) ) ;
#5993 =( NAMED_UNIT ( * ) PLANE_ANGLE_UNIT ( ) SI_UNIT ( $, .RADIAN. ) );
#5994 = AXIS2_PLACEMENT_3D ( 'NONE', #11749, #19225, #18793 ) ;
#5995 = DIRECTION ( 'NONE',  ( 0.000000000000000000, 0.000000000000000000, -1.000000000000000000 ) ) ;
#5996 = VECTOR ( 'NONE', #5432, 1000.000000000000000 ) ;
#5997 = CARTESIAN_POINT ( 'NONE',  ( 0.000000000000000000, 0.000000000000000000, 0.000000000000000000 ) ) ;
#5998 = AXIS2_PLACEMENT_3D ( 'NONE', #17048, #15327, #18894 ) ;
#5999 = CARTESIAN_POINT ( 'NONE',  ( 81.85249911436491743, 7.562528597612068045E-15, 0.000000000000000000 ) ) ;
#6000 = CARTESIAN_POINT ( 'NONE',  ( 29.00000000000000000, -29.50000000000000355, 12.00000000000000000 ) ) ;
#6001 = FACE_OUTER_BOUND ( 'NONE', #3203, .T. ) ;
#6002 = CIRCLE ( 'NONE', #21213, 1.499999999999998002 ) ;
#6003 = ORIENTED_EDGE ( 'NONE', *, *, #13421, .T. ) ;
#6004 = DIRECTION ( 'NONE',  ( -1.000000000000000000, 0.000000000000000000, 0.000000000000000000 ) ) ;
#6005 = CARTESIAN_POINT ( 'NONE',  ( -7.022953521754877748, -5.102474405760673015, 9.833165578109188232 ) ) ;
#6006 = CARTESIAN_POINT ( 'NONE',  ( 9.000000000000000000, 1.102182119232617714E-15, 0.9999999999999940048 ) ) ;
#6007 = DIRECTION ( 'NONE',  ( -0.000000000000000000, -0.000000000000000000, -1.000000000000000000 ) ) ;
#6008 = VERTEX_POINT ( 'NONE', #7712 ) ;
#6009 = CIRCLE ( 'NONE', #19674, 4.057500000000000107 ) ;
#6010 = CONICAL_SURFACE ( 'NONE', #20847, 0.9999999999999991118, 1.029744258676654090 ) ;
#6011 = ORIENTED_EDGE ( 'NONE', *, *, #8789, .F. ) ;
#6012 = EDGE_CURVE ( 'NONE', #10046, #2012, #22692, .T. ) ;
#6013 = ORIENTED_EDGE ( 'NONE', *, *, #13933, .T. ) ;
#6014 = LINE ( 'NONE', #19071, #1771 ) ;
#6015 = ADVANCED_FACE ( 'NONE', ( #5787 ), #7257, .F. ) ;
#6016 = CARTESIAN_POINT ( 'NONE',  ( -7.685661446561619314, -5.583959896779019161, -10.40674201446023339 ) ) ;
#6017 = EDGE_LOOP ( 'NONE', ( #12439, #19647, #16687, #10708 ) ) ;
#6018 = AXIS2_PLACEMENT_3D ( 'NONE', #3613, #22180, #22534 ) ;
#6019 = LINE ( 'NONE', #24080, #8101 ) ;
#6020 = VERTEX_POINT ( 'NONE', #5898 ) ;
#6021 = CARTESIAN_POINT ( 'NONE',  ( -8.512326165839379399, -4.253244381378425309, -3.501722726248814421 ) ) ;
#6022 = ORIENTED_EDGE ( 'NONE', *, *, #24074, .T. ) ;
#6023 = DIRECTION ( 'NONE',  ( -1.000000000000000000, -0.000000000000000000, -0.000000000000000000 ) ) ;
#6024 = CARTESIAN_POINT ( 'NONE',  ( -31.74999999999995737, 0.000000000000000000, 8.000000000000000000 ) ) ;
#6025 = DIRECTION ( 'NONE',  ( -1.000000000000000000, -0.000000000000000000, -0.000000000000000000 ) ) ;
#6026 = VECTOR ( 'NONE', #624, 1000.000000000000000 ) ;
#6027 = PRODUCT_DEFINITION_CONTEXT ( 'detailed design', #453, 'design' ) ;
#6028 = AXIS2_PLACEMENT_3D ( 'NONE', #22512, #20430, #9553 ) ;
#6029 = CARTESIAN_POINT ( 'NONE',  ( 0.7000000000000005107, 8.572527594031479353E-17, 4.000000000000000000 ) ) ;
#6030 = VERTEX_POINT ( 'NONE', #22392 ) ;
#6031 = FACE_OUTER_BOUND ( 'NONE', #7266, .T. ) ;
#6032 = DIRECTION ( 'NONE',  ( -0.000000000000000000, -0.000000000000000000, -1.000000000000000000 ) ) ;
#6033 = ORIENTED_EDGE ( 'NONE', *, *, #9294, .F. ) ;
#6034 = TOROIDAL_SURFACE ( 'NONE', #4489, 10.00000000000000888, 1.000000000000000000 ) ;
#6035 = ORIENTED_EDGE ( 'NONE', *, *, #21104, .T. ) ;
#6036 = CARTESIAN_POINT ( 'NONE',  ( -2.935661446561384391, -9.035036904804158553, 11.45958914175814414 ) ) ;
#6037 = EDGE_CURVE ( 'NONE', #22998, #14019, #19516, .T. ) ;
#6038 = EDGE_LOOP ( 'NONE', ( #15422, #9736, #22539, #23478 ) ) ;
#6039 = AXIS2_PLACEMENT_3D ( 'NONE', #12795, #16335, #9133 ) ;
#6040 = CARTESIAN_POINT ( 'NONE',  ( 9.500000000000200728, -3.086737114211976607, 5.959589141758144137 ) ) ;
#6041 = EDGE_CURVE ( 'NONE', #21399, #20932, #13721, .T. ) ;
#6042 = AXIS2_PLACEMENT_3D ( 'NONE', #3736, #10797, #1787 ) ;
#6043 = TOROIDAL_SURFACE ( 'NONE', #20468, 5.400000000000001243, 0.4000000000000000222 ) ;
#6044 = ORIENTED_EDGE ( 'NONE', *, *, #7448, .F. ) ;
#6045 = ORIENTED_EDGE ( 'NONE', *, *, #755, .F. ) ;
#6046 = EDGE_CURVE ( 'NONE', #4844, #12989, #11242, .T. ) ;
#6047 = CARTESIAN_POINT ( 'NONE',  ( 31.10231664966676846, -45.36128193761570770, 12.00000000000000000 ) ) ;
#6048 = CARTESIAN_POINT ( 'NONE',  ( 1.999999999999994449, -45.00000000000000000, 27.00000000000000000 ) ) ;
#6049 = EDGE_CURVE ( 'NONE', #7244, #898, #16869, .T. ) ;
#6050 = EDGE_CURVE ( 'NONE', #411, #18498, #5940, .T. ) ;
#6051 = DIRECTION ( 'NONE',  ( -0.000000000000000000, -0.000000000000000000, 1.000000000000000000 ) ) ;
#6052 = VERTEX_POINT ( 'NONE', #5429 ) ;
#6053 = CARTESIAN_POINT ( 'NONE',  ( -28.99999999999999645, -29.50000000000000000, -3.000000000000000000 ) ) ;
#6054 = CARTESIAN_POINT ( 'NONE',  ( 12.50000000000000178, 5.755434930044642846E-15, 2.500000000000000000 ) ) ;
#6055 = CARTESIAN_POINT ( 'NONE',  ( 74.57977184163763695, -5.000000000000000000, 6.123233995736775157E-16 ) ) ;
#6056 = TOROIDAL_SURFACE ( 'NONE', #19712, 12.73082370883260772, 1.500000000000000000 ) ;
#6057 = ORIENTED_EDGE ( 'NONE', *, *, #19185, .T. ) ;
#6058 = FACE_OUTER_BOUND ( 'NONE', #3823, .T. ) ;
#6059 = CYLINDRICAL_SURFACE ( 'NONE', #7476, 11.68650000001168721 ) ;
#6060 = AXIS2_PLACEMENT_3D ( 'NONE', #20740, #22573, #22471 ) ;
#6061 = ORIENTED_EDGE ( 'NONE', *, *, #19924, .F. ) ;
#6062 = CARTESIAN_POINT ( 'NONE',  ( 2.935661446562616295, -9.035036904803758873, -7.659589141758144315 ) ) ;
#6063 = VECTOR ( 'NONE', #19407, 1000.000000000000000 ) ;
#6064 = CARTESIAN_POINT ( 'NONE',  ( 16.82499651802897489, 7.532250541895348483, -5.808290850931483007 ) ) ;
#6065 = CIRCLE ( 'NONE', #19716, 4.249999999999996447 ) ;
#6066 = CARTESIAN_POINT ( 'NONE',  ( 0.000000000000000000, 0.000000000000000000, 0.000000000000000000 ) ) ;
#6067 = DIRECTION ( 'NONE',  ( 0.000000000000000000, 0.000000000000000000, 1.000000000000000000 ) ) ;
#6068 = ORIENTED_EDGE ( 'NONE', *, *, #9030, .T. ) ;
#6069 = ADVANCED_FACE ( 'NONE', ( #20310, #20667, #12972, #3947, #18481, #11131, #2120, #18606 ), #305, .F. ) ;
#6070 = ORIENTED_EDGE ( 'NONE', *, *, #21625, .T. ) ;
#6071 = CARTESIAN_POINT ( 'NONE',  ( 8.680847955710813579, 2.820578480814259326, 10.73316557810918503 ) ) ;
#6072 = AXIS2_PLACEMENT_3D ( 'NONE', #348, #2043, #3883 ) ;
#6073 = VERTEX_POINT ( 'NONE', #6257 ) ;
#6074 = LINE ( 'NONE', #19123, #19046 ) ;
#6075 = CONICAL_SURFACE ( 'NONE', #16979, 5.000000000000007994, 0.9599310885968855844 ) ;
#6076 = EDGE_CURVE ( 'NONE', #6155, #3367, #9662, .T. ) ;
#6077 = EDGE_CURVE ( 'NONE', #11604, #14761, #22988, .T. ) ;
#6078 = CARTESIAN_POINT ( 'NONE',  ( -5.871322893124554021, 8.081182679343978492, -10.75958914175814130 ) ) ;
#6080 = EDGE_CURVE ( 'NONE', #8089, #22930, #15406, .T. ) ;
#6079 = VECTOR ( 'NONE', #14699, 1000.000000000000000 ) ;
#6081 = VECTOR ( 'NONE', #9309, 1000.000000000000000 ) ;
#6082 = CARTESIAN_POINT ( 'NONE',  ( 6.507347684474039440, -5.969953219653517884, 12.49999999999999467 ) ) ;
#6083 = CARTESIAN_POINT ( 'NONE',  ( -31.74999999999995737, 6.123233995736767268E-16, -5.000000000000000888 ) ) ;
#6084 = CARTESIAN_POINT ( 'NONE',  ( -2.935661446561384391, -9.035036904804158553, 6.606742014460233570 ) ) ;
#6085 = EDGE_LOOP ( 'NONE', ( #11002, #22794, #18132, #19332, #13537 ) ) ;
#6086 = LINE ( 'NONE', #2300, #487 ) ;
#6087 = CARTESIAN_POINT ( 'NONE',  ( 62.36363636363636687, -4.172000000000000597, 5.616230220889771312E-16 ) ) ;
#6088 = AXIS2_PLACEMENT_3D ( 'NONE', #210, #7847, #15295 ) ;
#6089 = DIRECTION ( 'NONE',  ( 0.000000000000000000, -0.000000000000000000, 1.000000000000000000 ) ) ;
#6090 = DIRECTION ( 'NONE',  ( 1.000000000000000000, 0.000000000000000000, 0.000000000000000000 ) ) ;
#6091 = CARTESIAN_POINT ( 'NONE',  ( -16.81886298599062002, 7.518780870797757920, -5.825851398835387940 ) ) ;
#6092 = PRODUCT_DEFINITION_FORMATION_WITH_SPECIFIED_SOURCE ( 'ANY', '', #43, .NOT_KNOWN. ) ;
#6093 = AXIS2_PLACEMENT_3D ( 'NONE', #12480, #16380, #10299 ) ;
#6094 = DIRECTION ( 'NONE',  ( 0.000000000000000000, 0.000000000000000000, 1.000000000000000000 ) ) ;
#6095 = AXIS2_PLACEMENT_3D ( 'NONE', #16815, #13165, #264 ) ;
#6096 = ORIENTED_EDGE ( 'NONE', *, *, #16375, .F. ) ;
#6097 = VERTEX_POINT ( 'NONE', #23245 ) ;
#6098 = DIRECTION ( 'NONE',  ( 0.000000000000000000, 0.000000000000000000, 1.000000000000000000 ) ) ;
#6099 = CARTESIAN_POINT ( 'NONE',  ( -9.499999999999790390, -3.086737114213257804, 12.30674201446023197 ) ) ;
#6100 = ORIENTED_EDGE ( 'NONE', *, *, #20450, .T. ) ;
#6101 =( NAMED_UNIT ( * ) PLANE_ANGLE_UNIT ( ) SI_UNIT ( $, .RADIAN. ) );
#6102 = CARTESIAN_POINT ( 'NONE',  ( 87.96568270381690979, -9.244463733058732095E-30, 5.000000000000007994 ) ) ;
#6103 = DIRECTION ( 'NONE',  ( 1.000000000000000000, 0.000000000000000000, 0.000000000000000000 ) ) ;
#6104 = ORIENTED_EDGE ( 'NONE', *, *, #16386, .F. ) ;
#6105 = CARTESIAN_POINT ( 'NONE',  ( -20.85000000000000853, 15.04000000000000092, 27.00000000000000000 ) ) ;
#6106 = EDGE_CURVE ( 'NONE', #21210, #6921, #13698, .T. ) ;
#6107 = CARTESIAN_POINT ( 'NONE',  ( 7.524481829284253465, -4.467250836390667779, -12.49999999999999645 ) ) ;
#6108 = CARTESIAN_POINT ( 'NONE',  ( -10.00000000000000355, 15.50000000000000178, -2.999999999999999112 ) ) ;
#6109 = AXIS2_PLACEMENT_3D ( 'NONE', #12425, #21952, #10827 ) ;
#6110 = DIRECTION ( 'NONE',  ( 0.000000000000000000, -1.000000000000000000, 0.000000000000000000 ) ) ;
#6111 = ORIENTED_EDGE ( 'NONE', *, *, #22005, .F. ) ;
#6112 = CARTESIAN_POINT ( 'NONE',  ( -27.89784171216405895, 41.49349862090491570, -3.000000000000000000 ) ) ;
#6113 = ORIENTED_EDGE ( 'NONE', *, *, #3814, .F. ) ;
#6114 = DIRECTION ( 'NONE',  ( 0.000000000000000000, 0.000000000000000000, 1.000000000000000000 ) ) ;
#6115 = CIRCLE ( 'NONE', #16632, 6.050000000006051870 ) ;
#6116 = LINE ( 'NONE', #23845, #22348 ) ;
#6117 = DIRECTION ( 'NONE',  ( -1.000000000000000000, 0.000000000000000000, 0.000000000000000000 ) ) ;
#6118 = DIRECTION ( 'NONE',  ( -1.000000000000000000, 0.000000000000000000, 0.000000000000000000 ) ) ;
#6119 = FACE_OUTER_BOUND ( 'NONE', #23158, .T. ) ;
#6120 = EDGE_CURVE ( 'NONE', #6224, #1315, #17112, .T. ) ;
#6121 = DIRECTION ( 'NONE',  ( -0.000000000000000000, -0.000000000000000000, -1.000000000000000000 ) ) ;
#6122 = CYLINDRICAL_SURFACE ( 'NONE', #21184, 0.9999999999999991118 ) ;
#6123 = AXIS2_PLACEMENT_3D ( 'NONE', #3085, #19556, #3190 ) ;
#6124 = CARTESIAN_POINT ( 'NONE',  ( 6.809999908187194197E-13, -9.988891130263535700, -6.706742014460232326 ) ) ;
#6125 = ORIENTED_EDGE ( 'NONE', *, *, #21199, .F. ) ;
#6126 = DIRECTION ( 'NONE',  ( -0.000000000000000000, -0.000000000000000000, -1.000000000000000000 ) ) ;
#6127 = EDGE_CURVE ( 'NONE', #13972, #11452, #17617, .T. ) ;
#6128 = CARTESIAN_POINT ( 'NONE',  ( -7.022953521754877748, -5.102474405760673015, 11.83316557810918823 ) ) ;
#6129 = DIRECTION ( 'NONE',  ( 0.000000000000000000, -1.000000000000000000, 0.000000000000000000 ) ) ;
#6130 = SHAPE_REPRESENTATION ( 'Sleeve', ( #8005 ), #14253 ) ;
#6131 = ADVANCED_FACE ( 'NONE', ( #21147, #4204, #13464, #11615, #11494, #15780, #11863 ), #17597, .F. ) ;
#6132 = DIRECTION ( 'NONE',  ( -0.000000000000000000, -0.000000000000000000, -1.000000000000000000 ) ) ;
#6133 = EDGE_CURVE ( 'NONE', #10152, #22249, #10141, .T. ) ;
#6134 = ORIENTED_EDGE ( 'NONE', *, *, #2573, .T. ) ;
#6135 = ITEM_DEFINED_TRANSFORMATION ( 'NONE', 'NONE', #16583,  #8005 ) ;
#6136 = VERTEX_POINT ( 'NONE', #7822 ) ;
#6137 = CYLINDRICAL_SURFACE ( 'NONE', #10331, 13.72592346138681130 ) ;
#6138 = CARTESIAN_POINT ( 'NONE',  ( -2.935661446562617183, 9.035036904803758873, -9.806742014460233747 ) ) ;
#6139 = VERTEX_POINT ( 'NONE', #539 ) ;
#6140 = VERTEX_POINT ( 'NONE', #4318 ) ;
#6141 = DIRECTION ( 'NONE',  ( 1.000000000000000000, 0.000000000000000000, 0.000000000000000000 ) ) ;
#6142 = ORIENTED_EDGE ( 'NONE', *, *, #20185, .T. ) ;
#6143 = CARTESIAN_POINT ( 'NONE',  ( -9.453640352822144877, -1.087149405126631496, -3.499473001065527722 ) ) ;
#6144 = ORIENTED_EDGE ( 'NONE', *, *, #15201, .F. ) ;
#6145 = CARTESIAN_POINT ( 'NONE',  ( 23.00000000000000000, -2.110835303355385051, 14.05523051341064722 ) ) ;
#6146 = DIRECTION ( 'NONE',  ( -1.000000000000000000, 0.000000000000000000, -0.000000000000000000 ) ) ;
#6147 = LINE ( 'NONE', #22745, #23920 ) ;
#6148 = CARTESIAN_POINT ( 'NONE',  ( 12.50000000000000178, 5.755434930044642846E-15, 2.500000000000000000 ) ) ;
#6149 = ORIENTED_EDGE ( 'NONE', *, *, #13476, .F. ) ;
#6150 = PLANE ( 'NONE',  #16886 ) ;
#6151 = ADVANCED_FACE ( 'NONE', ( #19449 ), #15268, .F. ) ;
#6152 = CARTESIAN_POINT ( 'NONE',  ( -34.02499999999999858, 29.50000000000000000, -3.000000000000000000 ) ) ;
#6153 = EDGE_CURVE ( 'NONE', #11221, #13932, #7862, .T. ) ;
#6154 = CARTESIAN_POINT ( 'NONE',  ( 29.00000000000000000, 29.50000000000000355, 12.00000000000000000 ) ) ;
#6155 = VERTEX_POINT ( 'NONE', #2728 ) ;
#6156 = AXIS2_PLACEMENT_3D ( 'NONE', #14719, #5209, #5092 ) ;
#6157 = ORIENTED_EDGE ( 'NONE', *, *, #22390, .F. ) ;
#6158 = CARTESIAN_POINT ( 'NONE',  ( -6.233975306307046963E-13, 9.127583699786111282, 5.133165578109188054 ) ) ;
#6159 = EDGE_LOOP ( 'NONE', ( #19727, #1611, #8882, #21467 ) ) ;
#6160 = ORIENTED_EDGE ( 'NONE', *, *, #22266, .T. ) ;
#6161 = ORIENTED_EDGE ( 'NONE', *, *, #19982, .F. ) ;
#6162 = ORIENTED_EDGE ( 'NONE', *, *, #17355, .F. ) ;
#6163 = LINE ( 'NONE', #685, #18439 ) ;
#6164 = CARTESIAN_POINT ( 'NONE',  ( -6.233975306307046963E-13, 9.127583699786111282, -7.133165578109187166 ) ) ;
#6165 = CARTESIAN_POINT ( 'NONE',  ( -33.24999999999999289, 29.50000000000000000, 14.00000000000000178 ) ) ;
#6166 = EDGE_LOOP ( 'NONE', ( #12946, #11559, #15013, #1976, #3488 ) ) ;
#6167 = CARTESIAN_POINT ( 'NONE',  ( 41.50000000000000000, -28.80990663662250739, 12.00000000000000000 ) ) ;
#6168 = FACE_OUTER_BOUND ( 'NONE', #5042, .T. ) ;
#6169 = DIRECTION ( 'NONE',  ( 0.000000000000000000, -1.000000000000000000, 0.000000000000000000 ) ) ;
#6170 = DIRECTION ( 'NONE',  ( -0.000000000000000000, 1.000000000000000000, 0.000000000000000000 ) ) ;
#6171 = AXIS2_PLACEMENT_3D ( 'NONE', #7740, #15435, #20458 ) ;
#6172 = DIRECTION ( 'NONE',  ( 0.000000000000000000, 0.000000000000000000, -1.000000000000000000 ) ) ;
#6173 = AXIS2_PLACEMENT_3D ( 'NONE', #19327, #22871, #6141 ) ;
#6174 = VERTEX_POINT ( 'NONE', #8074 ) ;
#6175 = DIRECTION ( 'NONE',  ( 0.000000000000000000, 0.000000000000000000, 1.000000000000000000 ) ) ;
#6176 = MECHANICAL_DESIGN_GEOMETRIC_PRESENTATION_REPRESENTATION (  '', ( #20203 ), #6966 ) ;
#6177 = DIRECTION ( 'NONE',  ( -0.000000000000000000, 1.000000000000000000, -0.000000000000000000 ) ) ;
#6178 = ADVANCED_FACE ( 'NONE', ( #17236 ), #21031, .F. ) ;
#6179 = EDGE_LOOP ( 'NONE', ( #5004, #18699, #22611, #21546 ) ) ;
#6180 = CARTESIAN_POINT ( 'NONE',  ( 76.03431729618309021, 5.000000000000015099, 0.000000000000000000 ) ) ;
#6181 = CARTESIAN_POINT ( 'NONE',  ( -34.10000000000000142, -29.50000000000001066, 27.00000000000000000 ) ) ;
#6182 = EDGE_CURVE ( 'NONE', #21802, #13005, #492, .T. ) ;
#6183 = DIRECTION ( 'NONE',  ( -0.000000000000000000, -0.000000000000000000, -1.000000000000000000 ) ) ;
#6184 = ADVANCED_FACE ( 'NONE', ( #17367 ), #5158, .T. ) ;
#6185 = CARTESIAN_POINT ( 'NONE',  ( 7.022953521755574080, -5.102474405759714671, -6.433165578109188765 ) ) ;
#6186 = EDGE_CURVE ( 'NONE', #14475, #5909, #154, .T. ) ;
#6187 = ORIENTED_EDGE ( 'NONE', *, *, #1377, .F. ) ;
#6188 = SURFACE_STYLE_USAGE ( .BOTH. , #579 ) ;
#6189 = EDGE_LOOP ( 'NONE', ( #19328, #30, #10030, #11850, #19103, #8656 ) ) ;
#6190 = ORIENTED_EDGE ( 'NONE', *, *, #19217, .F. ) ;
#6191 = CARTESIAN_POINT ( 'NONE',  ( -2.682529543899159208, -8.255977015246598327, 8.033165578109189298 ) ) ;
#6192 = ORIENTED_EDGE ( 'NONE', *, *, #12726, .F. ) ;
#6193 = CARTESIAN_POINT ( 'NONE',  ( 0.000000000000000000, 0.000000000000000000, 0.000000000000000000 ) ) ;
#6194 = DIRECTION ( 'NONE',  ( 1.000000000000000000, 0.000000000000000000, 0.000000000000000000 ) ) ;
#6195 = ORIENTED_EDGE ( 'NONE', *, *, #6133, .F. ) ;
#6196 = DIRECTION ( 'NONE',  ( 0.000000000000000000, 0.000000000000000000, 1.000000000000000000 ) ) ;
#6197 = CARTESIAN_POINT ( 'NONE',  ( 7.685661446562381371, -5.583959896777971110, -11.00674201446023304 ) ) ;
#6198 = CARTESIAN_POINT ( 'NONE',  ( -35.99999999999993605, -60.00000000000000000, 12.50000000000000000 ) ) ;
#6199 = LINE ( 'NONE', #2661, #9538 ) ;
#6200 = VERTEX_POINT ( 'NONE', #16013 ) ;
#6201 = CARTESIAN_POINT ( 'NONE',  ( 0.2999999999999999334, 0.000000000000000000, 14.42592346043842433 ) ) ;
#6202 = FACE_OUTER_BOUND ( 'NONE', #16718, .T. ) ;
#6203 = EDGE_CURVE ( 'NONE', #14137, #17696, #12167, .T. ) ;
#6204 = CARTESIAN_POINT ( 'NONE',  ( 3.890962118697714531E-15, 15.50000000000000000, 19.70000000000000284 ) ) ;
#6205 = ORIENTED_EDGE ( 'NONE', *, *, #21676, .F. ) ;
#6206 = DIRECTION ( 'NONE',  ( 0.000000000000000000, -1.000000000000000000, 0.000000000000000000 ) ) ;
#6207 = DIRECTION ( 'NONE',  ( -1.000000000000000000, 0.000000000000000000, 0.000000000000000000 ) ) ;
#6208 = CARTESIAN_POINT ( 'NONE',  ( -15.78970982176773674, 5.581464347350853394, 7.700125654604360825 ) ) ;
#6209 = DIRECTION ( 'NONE',  ( 1.000000000000000000, 0.000000000000000000, 0.000000000000000000 ) ) ;
#6210 = EDGE_CURVE ( 'NONE', #14101, #10129, #4383, .T. ) ;
#6211 = EDGE_LOOP ( 'NONE', ( #6614, #18512, #3938, #4474 ) ) ;
#6212 = ADVANCED_FACE ( 'NONE', ( #21404 ), #6986, .F. ) ;
#6213 = ORIENTED_EDGE ( 'NONE', *, *, #8470, .F. ) ;
#6214 = CARTESIAN_POINT ( 'NONE',  ( 2.935661446562616295, -9.035036904803758873, 11.65958914175814520 ) ) ;
#6215 = CARTESIAN_POINT ( 'NONE',  ( -1.999999999999994449, 45.00000000000000000, 23.99999999999999645 ) ) ;
#6216 = ORIENTED_EDGE ( 'NONE', *, *, #930, .F. ) ;
#6217 = LINE ( 'NONE', #17684, #3283 ) ;
#6218 = CARTESIAN_POINT ( 'NONE',  ( 40.89823313241238623, -26.41789760203348081, 27.00000000000000000 ) ) ;
#6219 = CARTESIAN_POINT ( 'NONE',  ( 35.99999999999999289, 50.99999999999999289, 12.50000000000000000 ) ) ;
#6220 = DIRECTION ( 'NONE',  ( 1.000000000000000000, 0.000000000000000000, 0.000000000000000000 ) ) ;
#6221 = CARTESIAN_POINT ( 'NONE',  ( -2.999999999999999112, 6.000000000000000000, 80.99999999999998579 ) ) ;
#6222 = CARTESIAN_POINT ( 'NONE',  ( 23.00000000000000000, 0.000000000000000000, 0.000000000000000000 ) ) ;
#6223 = PLANE ( 'NONE',  #5530 ) ;
#6224 = VERTEX_POINT ( 'NONE', #14183 ) ;
#6225 = FACE_BOUND ( 'NONE', #10825, .T. ) ;
#6226 = ORIENTED_EDGE ( 'NONE', *, *, #4917, .F. ) ;
#6227 = CARTESIAN_POINT ( 'NONE',  ( -3.567126290007196499, -8.444559533753546177, 12.34121854105286786 ) ) ;
#6228 = CARTESIAN_POINT ( 'NONE',  ( 5.871322893124551356, -8.081182679343980269, 11.75958914175814485 ) ) ;
#6229 = CARTESIAN_POINT ( 'NONE',  ( -41.49999999999999289, 27.79189783386526358, -27.00000000000000000 ) ) ;
#6230 = VECTOR ( 'NONE', #16705, 1000.000000000000000 ) ;
#6231 = DIRECTION ( 'NONE',  ( -0.000000000000000000, -0.000000000000000000, -1.000000000000000000 ) ) ;
#6232 = FACE_OUTER_BOUND ( 'NONE', #12747, .T. ) ;
#6233 = EDGE_CURVE ( 'NONE', #1549, #11505, #21765, .T. ) ;
#6234 = CARTESIAN_POINT ( 'NONE',  ( -7.685661446562381371, 5.583959896777970222, -8.006742014460233037 ) ) ;
#6235 = CARTESIAN_POINT ( 'NONE',  ( -2.935661446562617183, 9.035036904803758873, 8.659589141758143427 ) ) ;
#6236 = EDGE_CURVE ( 'NONE', #18646, #7231, #3263, .T. ) ;
#6237 = ORIENTED_EDGE ( 'NONE', *, *, #6793, .F. ) ;
#6238 = CARTESIAN_POINT ( 'NONE',  ( 7.685661446561619314, 5.583959896779020049, -7.406742014460233392 ) ) ;
#6239 = ORIENTED_EDGE ( 'NONE', *, *, #3474, .F. ) ;
#6240 = DIRECTION ( 'NONE',  ( -1.000000000000000000, -1.224606353822377258E-16, -0.000000000000000000 ) ) ;
#6241 = CARTESIAN_POINT ( 'NONE',  ( -5.365059087798940141, -7.384370330707086261, 7.933165578109187877 ) ) ;
#6242 = CARTESIAN_POINT ( 'NONE',  ( 29.00000000000000000, 29.50000000000000000, -2.224999999999995204 ) ) ;
#6243 = DIRECTION ( 'NONE',  ( 0.000000000000000000, -0.4999999999999992784, 0.8660254037844390407 ) ) ;
#6244 = VERTEX_POINT ( 'NONE', #8688 ) ;
#6246 = ORIENTED_EDGE ( 'NONE', *, *, #12525, .F. ) ;
#6245 = CIRCLE ( 'NONE', #23427, 5.000000000000007994 ) ;
#6247 = ORIENTED_EDGE ( 'NONE', *, *, #22139, .T. ) ;
#6248 = EDGE_CURVE ( 'NONE', #14909, #5671, #7464, .T. ) ;
#6249 = CARTESIAN_POINT ( 'NONE',  ( -9.500000000000211386, 3.086737114211961064, -8.106742014460232681 ) ) ;
#6250 = ORIENTED_EDGE ( 'NONE', *, *, #6677, .F. ) ;
#6251 = EDGE_CURVE ( 'NONE', #19379, #16743, #6387, .T. ) ;
#6252 = CARTESIAN_POINT ( 'NONE',  ( 80.39795365981946418, -1.078520768856852078E-29, 5.000000000000007994 ) ) ;
#6253 = ORIENTED_EDGE ( 'NONE', *, *, #20841, .F. ) ;
#6254 = ADVANCED_FACE ( 'NONE', ( #19705 ), #20031, .T. ) ;
#6255 = EDGE_LOOP ( 'NONE', ( #14576, #287, #13685 ) ) ;
#6256 = DIRECTION ( 'NONE',  ( 0.000000000000000000, 0.000000000000000000, 1.000000000000000000 ) ) ;
#6257 = CARTESIAN_POINT ( 'NONE',  ( -0.6999999999999996225, 1.040949779275250140E-16, 0.000000000000000000 ) ) ;
#6258 = CARTESIAN_POINT ( 'NONE',  ( 0.000000000000000000, 0.000000000000000000, 0.000000000000000000 ) ) ;
#6259 =( BOUNDED_CURVE ( )  B_SPLINE_CURVE ( 2, ( #10161, #13260, #17619, #5836, #240, #20716, #11554, #13144, #4000, #15330, #19593 ),
 .UNSPECIFIED., .F., .T. ) 
 B_SPLINE_CURVE_WITH_KNOTS ( ( 3, 2, 2, 2, 2, 3 ),
 ( 0.7000000000000000666, 0.7200000000000000844, 0.7400000000000001021, 0.7600000000000000089, 0.7800000000000000266, 0.8000000000000000444 ),
 .UNSPECIFIED. ) 
 CURVE ( )  GEOMETRIC_REPRESENTATION_ITEM ( )  RATIONAL_B_SPLINE_CURVE ( ( 0.9999999999999997780, 0.9510565162951537532, 1.000000000000000000, 0.9510565162951535312, 1.000000000000000000, 0.9510565162951535312, 1.000000000000000000, 0.9510565162951535312, 1.000000000000000000, 0.9510565162951535312, 1.000000000000000000 ) ) 
 REPRESENTATION_ITEM ( '' )  );
#6260 = DIRECTION ( 'NONE',  ( -0.5735764363510519326, 0.8191520442889876907, 1.003171929053519816E-16 ) ) ;
#6261 = ORIENTED_EDGE ( 'NONE', *, *, #5308, .T. ) ;
#6262 = FACE_OUTER_BOUND ( 'NONE', #7918, .T. ) ;
#6263 = DIRECTION ( 'NONE',  ( -0.000000000000000000, -0.000000000000000000, -1.000000000000000000 ) ) ;
#6264 = CARTESIAN_POINT ( 'NONE',  ( 3.890962118697714531E-15, 15.50000000000000000, 12.50000000000000000 ) ) ;
#6265 = ORIENTED_EDGE ( 'NONE', *, *, #7379, .F. ) ;
#6266 = VERTEX_POINT ( 'NONE', #1266 ) ;
#6267 = CARTESIAN_POINT ( 'NONE',  ( 9.500000000000000000, 6.470877716354879437E-13, 10.05958914175814378 ) ) ;
#6268 = ORIENTED_EDGE ( 'NONE', *, *, #4520, .F. ) ;
#6269 = ORIENTED_EDGE ( 'NONE', *, *, #19806, .F. ) ;
#6270 = EDGE_LOOP ( 'NONE', ( #22100, #402, #5407, #9902 ) ) ;
#6271 = VERTEX_POINT ( 'NONE', #8925 ) ;
#6272 = VERTEX_POINT ( 'NONE', #17864 ) ;
#6273 = ORIENTED_EDGE ( 'NONE', *, *, #13659, .F. ) ;
#6274 = DIRECTION ( 'NONE',  ( -1.000000000000000000, -1.224606353822377258E-16, -0.000000000000000000 ) ) ;
#6275 = CARTESIAN_POINT ( 'NONE',  ( -8.680847955711007202, -5.923547351154968927E-13, -3.633165578109188054 ) ) ;
#6276 = EDGE_CURVE ( 'NONE', #14424, #6139, #19571, .T. ) ;
#6277 = PRESENTATION_LAYER_ASSIGNMENT (  '', '', ( #16787 ) ) ;
#6278 = ORIENTED_EDGE ( 'NONE', *, *, #8969, .F. ) ;
#6279 = DIRECTION ( 'NONE',  ( 0.000000000000000000, 0.000000000000000000, 1.000000000000000000 ) ) ;
#6280 = LINE ( 'NONE', #10048, #15825 ) ;
#6281 = DIRECTION ( 'NONE',  ( 0.000000000000000000, -1.000000000000000000, 0.000000000000000000 ) ) ;
#6282 = EDGE_CURVE ( 'NONE', #13474, #12890, #12600, .T. ) ;
#6283 = DIRECTION ( 'NONE',  ( -1.000000000000000000, -0.000000000000000000, -0.000000000000000000 ) ) ;
#6284 = CARTESIAN_POINT ( 'NONE',  ( 0.7000000000000005107, 1.040949779275250633E-16, 4.000000000000000000 ) ) ;
#6285 = AXIS2_PLACEMENT_3D ( 'NONE', #12770, #18634, #10809 ) ;
#6286 = EDGE_LOOP ( 'NONE', ( #8917, #5972, #8327, #21855 ) ) ;
#6287 = DIRECTION ( 'NONE',  ( 0.000000000000000000, 0.000000000000000000, -1.000000000000000000 ) ) ;
#6288 = DIRECTION ( 'NONE',  ( -0.000000000000000000, -0.000000000000000000, -1.000000000000000000 ) ) ;
#6289 = ORIENTED_EDGE ( 'NONE', *, *, #16306, .F. ) ;
#6290 = DIRECTION ( 'NONE',  ( 0.000000000000000000, 0.000000000000000000, -1.000000000000000000 ) ) ;
#6291 = CARTESIAN_POINT ( 'NONE',  ( -28.99999999999999645, -29.50000000000000000, -3.000000000000000000 ) ) ;
#6292 = CARTESIAN_POINT ( 'NONE',  ( 0.000000000000000000, 15.23000000000000220, -27.00000000000000000 ) ) ;
#6293 = CARTESIAN_POINT ( 'NONE',  ( -2.682529543900285862, 8.255977015246234174, -5.233165578109188587 ) ) ;
#6294 = ORIENTED_EDGE ( 'NONE', *, *, #17541, .T. ) ;
#6295 = DIRECTION ( 'NONE',  ( -0.5735764363510519326, 0.8191520442889876907, 1.003171929053519816E-16 ) ) ;
#6296 = EDGE_LOOP ( 'NONE', ( #3923, #3457, #7999, #21278, #7771 ) ) ;
#6297 = ORIENTED_EDGE ( 'NONE', *, *, #11164, .T. ) ;
#6298 = AXIS2_PLACEMENT_3D ( 'NONE', #21216, #1208, #11925 ) ;
#6299 = CARTESIAN_POINT ( 'NONE',  ( -8.680847955711200825, 2.820578480813073607, 11.53316557810918574 ) ) ;
#6300 = AXIS2_PLACEMENT_3D ( 'NONE', #22261, #5673, #16284 ) ;
#6301 = ORIENTED_EDGE ( 'NONE', *, *, #4905, .F. ) ;
#6302 = SHAPE_REPRESENTATION_RELATIONSHIP ( 'NONE' , 'NONE' ,  #1013, #10480 ) ;
#6303 = CARTESIAN_POINT ( 'NONE',  ( 1.000000000000000222, 0.000000000000000000, 0.2999999999999990452 ) ) ;
#6304 = ORIENTED_EDGE ( 'NONE', *, *, #18409, .F. ) ;
#6305 = CARTESIAN_POINT ( 'NONE',  ( -9.500000000000211386, 3.086737114211961064, -10.95958914175814414 ) ) ;
#6306 = CARTESIAN_POINT ( 'NONE',  ( -9.499999999999799272, -3.086737114213243593, -10.30674201446023019 ) ) ;
#6307 = DIRECTION ( 'NONE',  ( 1.000000000000000000, 0.000000000000000000, 0.000000000000000000 ) ) ;
#6308 = CARTESIAN_POINT ( 'NONE',  ( 6.809999908187194197E-13, -9.988891130263535700, 6.706742014460232326 ) ) ;
#6309 = ADVANCED_FACE ( 'NONE', ( #10633 ), #21647, .F. ) ;
#6310 = EDGE_CURVE ( 'NONE', #10172, #23824, #16823, .T. ) ;
#6311 = ORIENTED_EDGE ( 'NONE', *, *, #6436, .F. ) ;
#6312 = CARTESIAN_POINT ( 'NONE',  ( -42.62132034355961707, -25.48082444701823235, -4.874844804309807125E-16 ) ) ;
#6313 = CARTESIAN_POINT ( 'NONE',  ( 23.00000000000000000, -10.66755332433025139, 4.772587172891002538 ) ) ;
#6314 = AXIS2_PLACEMENT_3D ( 'NONE', #3864, #11159, #5813 ) ;
#6315 = VECTOR ( 'NONE', #19955, 1000.000000000000000 ) ;
#6316 = AXIS2_PLACEMENT_3D ( 'NONE', #18436, #1726, #16598 ) ;
#6317 = DIRECTION ( 'NONE',  ( -1.000000000000000000, 0.000000000000000000, 0.000000000000000000 ) ) ;
#6318 = CIRCLE ( 'NONE', #1658, 8.000000000000003553 ) ;
#6319 = ORIENTED_EDGE ( 'NONE', *, *, #1696, .F. ) ;
#6320 = DIRECTION ( 'NONE',  ( 1.000000000000000000, 0.000000000000000000, 0.000000000000000000 ) ) ;
#6321 = CARTESIAN_POINT ( 'NONE',  ( 40.00000000000000000, 0.000000000000000000, 0.000000000000000000 ) ) ;
#6322 = VECTOR ( 'NONE', #7672, 1000.000000000000000 ) ;
#6323 = CARTESIAN_POINT ( 'NONE',  ( 0.000000000000000000, 0.000000000000000000, 0.000000000000000000 ) ) ;
#6324 = AXIS2_PLACEMENT_3D ( 'NONE', #20054, #5052, #2849 ) ;
#6325 = CIRCLE ( 'NONE', #9817, 4.999999999999997335 ) ;
#6326 = CARTESIAN_POINT ( 'NONE',  ( 0.000000000000000000, -15.03999999999999915, -25.00000000000000000 ) ) ;
#6327 = VERTEX_POINT ( 'NONE', #3334 ) ;
#6328 = ORIENTED_EDGE ( 'NONE', *, *, #2601, .F. ) ;
#6329 = ORIENTED_EDGE ( 'NONE', *, *, #10999, .T. ) ;
#6330 = DIRECTION ( 'NONE',  ( -1.000000000000000000, 0.000000000000000000, 0.000000000000000000 ) ) ;
#6331 = CARTESIAN_POINT ( 'NONE',  ( 2.935661446562616295, -9.035036904803758873, 12.80674201446023375 ) ) ;
#6332 = ORIENTED_EDGE ( 'NONE', *, *, #1464, .T. ) ;
#6333 = PLANE ( 'NONE',  #4870 ) ;
#6334 = ADVANCED_FACE ( 'NONE', ( #8461 ), #23369, .F. ) ;
#6335 = DIRECTION ( 'NONE',  ( -1.000000000000000000, -0.000000000000000000, -0.000000000000000000 ) ) ;
#6336 = CARTESIAN_POINT ( 'NONE',  ( 61.48886275072855057, 7.562528597612068045E-15, 0.000000000000000000 ) ) ;
#6337 = AXIS2_PLACEMENT_3D ( 'NONE', #4875, #15841, #1092 ) ;
#6338 = AXIS2_PLACEMENT_3D ( 'NONE', #21985, #5269, #18209 ) ;
#6339 = DIRECTION ( 'NONE',  ( 1.000000000000000000, 0.000000000000000000, 0.000000000000000000 ) ) ;
#6340 = AXIS2_PLACEMENT_3D ( 'NONE', #14743, #22206, #7186 ) ;
#6341 = AXIS2_PLACEMENT_3D ( 'NONE', #22238, #12714, #1618 ) ;
#6342 = ADVANCED_FACE ( 'NONE', ( #12233, #10515 ), #2982, .F. ) ;
#6343 = AXIS2_PLACEMENT_3D ( 'NONE', #17198, #20197, #17082 ) ;
#6344 = FACE_OUTER_BOUND ( 'NONE', #1096, .T. ) ;
#6345 = DIRECTION ( 'NONE',  ( 1.000000000000000000, 0.000000000000000000, 0.000000000000000000 ) ) ;
#6346 = EDGE_CURVE ( 'NONE', #2739, #23101, #1961, .T. ) ;
#6347 = ADVANCED_FACE ( 'NONE', ( #18582 ), #16618, .F. ) ;
#6348 = EDGE_CURVE ( 'NONE', #8876, #22006, #24060, .T. ) ;
#6349 = DIRECTION ( 'NONE',  ( -0.000000000000000000, -0.000000000000000000, 1.000000000000000000 ) ) ;
#6350 = ORIENTED_EDGE ( 'NONE', *, *, #12830, .F. ) ;
#6351 = CARTESIAN_POINT ( 'NONE',  ( 81.27272727272728048, 4.172000000000015696, 0.000000000000000000 ) ) ;
#6352 = ORIENTED_EDGE ( 'NONE', *, *, #12398, .F. ) ;
#6353 = FACE_OUTER_BOUND ( 'NONE', #22655, .T. ) ;
#6354 = CARTESIAN_POINT ( 'NONE',  ( -0.9419320875194652221, -9.063431280198074091, 12.39598011385684373 ) ) ;
#6355 = CARTESIAN_POINT ( 'NONE',  ( 40.77574956473004164, -27.49633847812775755, 11.00000000000000000 ) ) ;
#6356 =( NAMED_UNIT ( * ) SI_UNIT ( $, .STERADIAN. ) SOLID_ANGLE_UNIT ( ) );
#6357 = AXIS2_PLACEMENT_3D ( 'NONE', #8358, #1064, #21429 ) ;
#6358 = LINE ( 'NONE', #6850, #18327 ) ;
#6359 = ORIENTED_EDGE ( 'NONE', *, *, #5606, .F. ) ;
#6360 = AXIS2_PLACEMENT_3D ( 'NONE', #6323, #1098, #11795 ) ;
#6361 = LINE ( 'NONE', #13804, #3624 ) ;
#6362 = AXIS2_PLACEMENT_3D ( 'NONE', #3467, #10531, #14087 ) ;
#6363 = CARTESIAN_POINT ( 'NONE',  ( 24.75000000000000000, 29.50000000000000000, -2.224999999999995204 ) ) ;
#6364 = VECTOR ( 'NONE', #18976, 1000.000000000000000 ) ;
#6365 = EDGE_LOOP ( 'NONE', ( #8547, #10066, #19782, #106 ) ) ;
#6366 = CARTESIAN_POINT ( 'NONE',  ( 2.935661446562616295, -9.035036904803758873, -4.806742014460232859 ) ) ;
#6367 = VERTEX_POINT ( 'NONE', #20175 ) ;
#6368 = CARTESIAN_POINT ( 'NONE',  ( -31.10231664966676135, -45.36128193761570770, 27.00000000000000000 ) ) ;
#6369 = CARTESIAN_POINT ( 'NONE',  ( -7.022953521755574080, 5.102474405759713783, 11.43316557810918965 ) ) ;
#6370 = AXIS2_PLACEMENT_3D ( 'NONE', #17189, #17443, #623 ) ;
#6371 = LINE ( 'NONE', #8173, #21706 ) ;
#6372 = EDGE_CURVE ( 'NONE', #12689, #13734, #20640, .T. ) ;
#6373 = DIRECTION ( 'NONE',  ( 0.000000000000000000, 0.000000000000000000, -1.000000000000000000 ) ) ;
#6374 =( REPRESENTATION_RELATIONSHIP ('NONE','NONE', #21748, #15960 ) REPRESENTATION_RELATIONSHIP_WITH_TRANSFORMATION ( #13084 )SHAPE_REPRESENTATION_RELATIONSHIP( ) );
#6375 = EDGE_LOOP ( 'NONE', ( #17037, #23118 ) ) ;
#6376 = CIRCLE ( 'NONE', #5206, 5.000000000000007994 ) ;
#6377 = ORIENTED_EDGE ( 'NONE', *, *, #11233, .F. ) ;
#6378 = DIRECTION ( 'NONE',  ( -0.000000000000000000, -0.000000000000000000, -1.000000000000000000 ) ) ;
#6379 = EDGE_CURVE ( 'NONE', #12712, #17488, #14667, .T. ) ;
#6380 = AXIS2_PLACEMENT_3D ( 'NONE', #1619, #18457, #1400 ) ;
#6381 = AXIS2_PLACEMENT_3D ( 'NONE', #2621, #21152, #19087 ) ;
#6382 = CARTESIAN_POINT ( 'NONE',  ( 9.499999999999790390, 3.086737114213260025, -11.30674201446023019 ) ) ;
#6383 = ORIENTED_EDGE ( 'NONE', *, *, #10862, .F. ) ;
#6384 = VECTOR ( 'NONE', #7734, 1000.000000000000114 ) ;
#6385 = EDGE_LOOP ( 'NONE', ( #22774, #15050, #23273, #10952 ) ) ;
#6386 = CARTESIAN_POINT ( 'NONE',  ( -6.218841404285884167, -6.822046258104109029, -12.27696493876690909 ) ) ;
#6387 = CIRCLE ( 'NONE', #23150, 11.00000000000000711 ) ;
#6388 = CIRCLE ( 'NONE', #156, 1.500000000000001332 ) ;
#6389 = FACE_BOUND ( 'NONE', #22028, .T. ) ;
#6390 = AXIS2_PLACEMENT_3D ( 'NONE', #23007, #8097, #7736 ) ;
#6391 = DIRECTION ( 'NONE',  ( -0.000000000000000000, -0.000000000000000000, -1.000000000000000000 ) ) ;
#6392 = EDGE_LOOP ( 'NONE', ( #2954, #8371, #3616, #15892 ) ) ;
#6393 = DIRECTION ( 'NONE',  ( -1.000000000000000000, -1.224606353822377258E-16, -0.000000000000000000 ) ) ;
#6394 = DIRECTION ( 'NONE',  ( 1.000000000000000000, -0.000000000000000000, -0.000000000000000000 ) ) ;
#6395 = CARTESIAN_POINT ( 'NONE',  ( -36.00000000000000711, -51.00000000000000711, 12.50000000000000000 ) ) ;
#6396 = CARTESIAN_POINT ( 'NONE',  ( 41.00000000000000000, -5.000000000000015099, 9.500000000000000000 ) ) ;
#6397 = ORIENTED_EDGE ( 'NONE', *, *, #8637, .T. ) ;
#6398 = DIRECTION ( 'NONE',  ( -0.7071067811865574537, 0.000000000000000000, -0.7071067811865376918 ) ) ;
#6399 = DIRECTION ( 'NONE',  ( 0.000000000000000000, 0.000000000000000000, -1.000000000000000000 ) ) ;
#6400 = DIRECTION ( 'NONE',  ( -0.000000000000000000, -0.000000000000000000, -1.000000000000000000 ) ) ;
#6401 = ORIENTED_EDGE ( 'NONE', *, *, #6372, .F. ) ;
#6402 = EDGE_LOOP ( 'NONE', ( #10037, #1521, #12750, #19461, #12, #21298 ) ) ;
#6403 = CARTESIAN_POINT ( 'NONE',  ( -9.500000000000000000, -6.482511860946779655E-13, 9.059589141758143782 ) ) ;
#6404 = ORIENTED_EDGE ( 'NONE', *, *, #9965, .T. ) ;
#6405 = ORIENTED_EDGE ( 'NONE', *, *, #251, .F. ) ;
#6406 = ADVANCED_FACE ( 'NONE', ( #1860 ), #11101, .F. ) ;
#6407 = AXIS2_PLACEMENT_3D ( 'NONE', #8928, #9050, #16368 ) ;
#6408 = ORIENTED_EDGE ( 'NONE', *, *, #18251, .F. ) ;
#6409 = CIRCLE ( 'NONE', #12626, 5.000000000000007994 ) ;
#6410 = CIRCLE ( 'NONE', #2521, 4.249999999999996447 ) ;
#6411 = AXIS2_PLACEMENT_3D ( 'NONE', #6820, #23422, #5001 ) ;
#6412 = ORIENTED_EDGE ( 'NONE', *, *, #22227, .F. ) ;
#6413 = DIRECTION ( 'NONE',  ( 0.000000000000000000, 0.000000000000000000, -1.000000000000000000 ) ) ;
#6414 = DIRECTION ( 'NONE',  ( -1.000000000000000000, -0.000000000000000000, -0.000000000000000000 ) ) ;
#6415 = ADVANCED_FACE ( 'NONE', ( #18804 ), #9280, .T. ) ;
#6416 = CARTESIAN_POINT ( 'NONE',  ( -14.51962751333974033, -3.765689428759031010, -8.721787840009202597 ) ) ;
#6417 = FACE_OUTER_BOUND ( 'NONE', #12658, .T. ) ;
#6418 = ORIENTED_EDGE ( 'NONE', *, *, #21397, .F. ) ;
#6419 = CARTESIAN_POINT ( 'NONE',  ( -17.52854577772372835, -9.313395544511447355, 1.935253206038904716 ) ) ;
#6420 = DIRECTION ( 'NONE',  ( 1.000000000000000000, 0.000000000000000000, 0.000000000000000000 ) ) ;
#6421 = PLANE ( 'NONE',  #4811 ) ;
#6422 = DIRECTION ( 'NONE',  ( -0.000000000000000000, -0.000000000000000000, 1.000000000000000000 ) ) ;
#6423 = ORIENTED_EDGE ( 'NONE', *, *, #23556, .T. ) ;
#6424 = CARTESIAN_POINT ( 'NONE',  ( -20.85000000000000853, 15.04000000000000092, -25.00000000000000000 ) ) ;
#6425 = CARTESIAN_POINT ( 'NONE',  ( 7.685661446562381371, -5.583959896777971110, 7.859589141758143604 ) ) ;
#6426 = MECHANICAL_DESIGN_GEOMETRIC_PRESENTATION_REPRESENTATION (  '', ( #12636 ), #15344 ) ;
#6427 = CIRCLE ( 'NONE', #4890, 4.172000000000008590 ) ;
#6428 = ORIENTED_EDGE ( 'NONE', *, *, #10572, .T. ) ;
#6429 = CYLINDRICAL_SURFACE ( 'NONE', #21023, 6.050000000006051870 ) ;
#6430 = DIRECTION ( 'NONE',  ( -0.000000000000000000, -0.000000000000000000, 1.000000000000000000 ) ) ;
#6431 = VECTOR ( 'NONE', #10966, 1000.000000000000000 ) ;
#6432 = DIRECTION ( 'NONE',  ( 0.000000000000000000, 0.000000000000000000, 1.000000000000000000 ) ) ;
#6433 = VECTOR ( 'NONE', #2782, 1000.000000000000000 ) ;
#6434 = CARTESIAN_POINT ( 'NONE',  ( 14.91624121966758842, 1.615102390220948037, 9.367332145225617523 ) ) ;
#6435 = CARTESIAN_POINT ( 'NONE',  ( 7.022953521754877748, 5.102474405760673903, -6.833165578109188232 ) ) ;
#6436 = EDGE_CURVE ( 'NONE', #5218, #1117, #4815, .T. ) ;
#6437 = AXIS2_PLACEMENT_3D ( 'NONE', #12146, #4622, #21693 ) ;
#6438 = CARTESIAN_POINT ( 'NONE',  ( -19.84999999999999787, -16.67999999999985761, 13.50000000000000178 ) ) ;
#6439 = ORIENTED_EDGE ( 'NONE', *, *, #12129, .F. ) ;
#6440 = EDGE_LOOP ( 'NONE', ( #18260, #2498, #10145, #18431, #17385 ) ) ;
#6441 = ADVANCED_FACE ( 'NONE', ( #31 ), #16837, .F. ) ;
#6442 = ORIENTED_EDGE ( 'NONE', *, *, #8739, .F. ) ;
#6443 = DIRECTION ( 'NONE',  ( 0.9999999089179142375, -0.0004268069395492307943, -2.168404344971001646E-19 ) ) ;
#6444 = EDGE_CURVE ( 'NONE', #21692, #20393, #18456, .T. ) ;
#6445 = DIRECTION ( 'NONE',  ( 0.000000000000000000, 1.000000000000000000, 0.000000000000000000 ) ) ;
#6446 = ORIENTED_EDGE ( 'NONE', *, *, #16933, .T. ) ;
#6447 = LINE ( 'NONE', #12399, #9152 ) ;
#6448 = CARTESIAN_POINT ( 'NONE',  ( 44.99999999999998579, -51.00000000000000711, 12.50000000000000000 ) ) ;
#6449 = AXIS2_PLACEMENT_3D ( 'NONE', #20722, #11791, #4143 ) ;
#6450 = CARTESIAN_POINT ( 'NONE',  ( 3.000000000000003109, 8.485281374238567764, 98.99999999999998579 ) ) ;
#6451 = DIRECTION ( 'NONE',  ( -1.000000000000000000, 0.000000000000000000, 0.000000000000000000 ) ) ;
#6452 = DIRECTION ( 'NONE',  ( 1.000000000000000000, 0.000000000000000000, 0.000000000000000000 ) ) ;
#6453 = FACE_OUTER_BOUND ( 'NONE', #14229, .T. ) ;
#6454 = VECTOR ( 'NONE', #11835, 1000.000000000000000 ) ;
#6455 = CIRCLE ( 'NONE', #22049, 1.499999999999999556 ) ;
#6456 = CARTESIAN_POINT ( 'NONE',  ( -40.23082370883260239, 29.50000000000000711, -1.500000000000000000 ) ) ;
#6457 = DIRECTION ( 'NONE',  ( 0.5654966663575753394, -0.8247505806839234843, 0.000000000000000000 ) ) ;
#6458 = DIRECTION ( 'NONE',  ( -1.000000000000000000, -0.000000000000000000, -0.000000000000000000 ) ) ;
#6459 = CARTESIAN_POINT ( 'NONE',  ( 73.12522638709218370, 7.562528597612068045E-15, 0.000000000000000000 ) ) ;
#6460 = DIRECTION ( 'NONE',  ( -0.000000000000000000, -0.000000000000000000, -1.000000000000000000 ) ) ;
#6461 = DIRECTION ( 'NONE',  ( -0.000000000000000000, -0.000000000000000000, 1.000000000000000000 ) ) ;
#6462 = ORIENTED_EDGE ( 'NONE', *, *, #10988, .T. ) ;
#6463 = CARTESIAN_POINT ( 'NONE',  ( -5.871322893124554021, 8.081182679343978492, -11.90674201446023339 ) ) ;
#6464 = ORIENTED_EDGE ( 'NONE', *, *, #20894, .F. ) ;
#6465 = CIRCLE ( 'NONE', #18535, 1.500000000000000000 ) ;
#6466 = ORIENTED_EDGE ( 'NONE', *, *, #15108, .T. ) ;
#6467 = CARTESIAN_POINT ( 'NONE',  ( -7.685661446561619314, -5.583959896779019161, 7.259589141758143960 ) ) ;
#6468 = EDGE_CURVE ( 'NONE', #14984, #16640, #13743, .T. ) ;
#6469 = CYLINDRICAL_SURFACE ( 'NONE', #18310, 9.999999999999998224 ) ;
#6470 = EDGE_CURVE ( 'NONE', #430, #4506, #22133, .T. ) ;
#6471 = AXIS2_PLACEMENT_3D ( 'NONE', #1177, #4968, #17887 ) ;
#6472 = EDGE_LOOP ( 'NONE', ( #9918, #23379, #22656 ) ) ;
#6473 = DIRECTION ( 'NONE',  ( 0.000000000000000000, -1.000000000000000000, 0.000000000000000000 ) ) ;
#6474 = CARTESIAN_POINT ( 'NONE',  ( 18.50000000000000000, 15.23000000000000398, 27.00000000000000000 ) ) ;
#6475 = EDGE_LOOP ( 'NONE', ( #2509, #6383, #21369, #4089, #15299 ) ) ;
#6476 = CARTESIAN_POINT ( 'NONE',  ( -9.500000000000000000, -6.482511860946779655E-13, 3.059589141758143338 ) ) ;
#6477 = CARTESIAN_POINT ( 'NONE',  ( -6.822232771736904647E-13, 9.988891130263535700, 6.559589141758143782 ) ) ;
#6478 = CARTESIAN_POINT ( 'NONE',  ( 5.021738411795491075, -7.393327316361923529, -12.50000000000000178 ) ) ;
#6479 = CARTESIAN_POINT ( 'NONE',  ( 33.99999999999998579, -1.387778780781445676E-14, 10.49999999999999822 ) ) ;
#6480 = CARTESIAN_POINT ( 'NONE',  ( 33.25000000000000000, -29.50000000000000000, -3.000000000000000000 ) ) ;
#6481 = AXIS2_PLACEMENT_3D ( 'NONE', #22284, #22532, #18735 ) ;
#6482 = DIRECTION ( 'NONE',  ( 0.000000000000000000, 0.000000000000000000, -1.000000000000000000 ) ) ;
#6483 = EDGE_LOOP ( 'NONE', ( #6162, #2951, #19248, #12513, #5555 ) ) ;
#6484 = CIRCLE ( 'NONE', #13095, 18.50000000000000000 ) ;
#6485 = ORIENTED_EDGE ( 'NONE', *, *, #11233, .T. ) ;
#6486 = DIRECTION ( 'NONE',  ( -1.000000000000000000, -1.224606353822377258E-16, -0.000000000000000000 ) ) ;
#6487 = CYLINDRICAL_SURFACE ( 'NONE', #16109, 17.87500000001787726 ) ;
#6488 = CYLINDRICAL_SURFACE ( 'NONE', #17637, 8.000000000000003553 ) ;
#6489 = DIRECTION ( 'NONE',  ( 1.000000000000000000, 2.600433232233976523E-16, 0.000000000000000000 ) ) ;
#6490 = AXIS2_PLACEMENT_3D ( 'NONE', #10847, #13541, #9490 ) ;
#6491 = EDGE_CURVE ( 'NONE', #18644, #13723, #20284, .T. ) ;
#6492 = DIRECTION ( 'NONE',  ( 1.000000000000000000, 0.000000000000000000, 0.000000000000000000 ) ) ;
#6493 = ORIENTED_EDGE ( 'NONE', *, *, #11636, .F. ) ;
#6494 = FACE_OUTER_BOUND ( 'NONE', #21879, .T. ) ;
#6495 = CARTESIAN_POINT ( 'NONE',  ( -1.999999999999994449, -45.00000000000000000, 3.000000000000002665 ) ) ;
#6496 = ADVANCED_FACE ( 'NONE', ( #3806, #22489 ), #9168, .F. ) ;
#6497 = ORIENTED_EDGE ( 'NONE', *, *, #2665, .F. ) ;
#6498 = CARTESIAN_POINT ( 'NONE',  ( 5.871322893123449127, 8.081182679344781405, -5.506742014460233925 ) ) ;
#6499 = ORIENTED_EDGE ( 'NONE', *, *, #3556, .T. ) ;
#6500 = DIRECTION ( 'NONE',  ( -0.000000000000000000, 0.000000000000000000, 1.000000000000000000 ) ) ;
#6501 = CARTESIAN_POINT ( 'NONE',  ( 2.682529543900284974, -8.255977015246234174, 8.233165578109190363 ) ) ;
#6502 = EDGE_CURVE ( 'NONE', #7988, #4702, #5959, .T. ) ;
#6503 = EDGE_CURVE ( 'NONE', #13734, #23514, #9063, .T. ) ;
#6504 = AXIS2_PLACEMENT_3D ( 'NONE', #9526, #22495, #11471 ) ;
#6505 = DIRECTION ( 'NONE',  ( -1.000000000000000000, 0.000000000000000000, -0.000000000000000000 ) ) ;
#6506 = AXIS2_PLACEMENT_3D ( 'NONE', #17415, #710, #2653 ) ;
#6507 = CIRCLE ( 'NONE', #16602, 7.999999999999986677 ) ;
#6508 = CARTESIAN_POINT ( 'NONE',  ( 0.000000000000000000, 4.685197434473818312, -1.301042606982605321E-15 ) ) ;
#6509 = CARTESIAN_POINT ( 'NONE',  ( -9.499999999999799272, -3.086737114213243593, 5.159589141758141650 ) ) ;
#6510 = AXIS2_PLACEMENT_3D ( 'NONE', #5240, #8773, #8995 ) ;
#6511 = ORIENTED_EDGE ( 'NONE', *, *, #19154, .F. ) ;
#6512 = CARTESIAN_POINT ( 'NONE',  ( 40.00000000000000000, -29.49999999999999645, 0.000000000000000000 ) ) ;
#6513 = CARTESIAN_POINT ( 'NONE',  ( 2.935661446562616295, -9.035036904803758873, -10.80674201446023197 ) ) ;
#6514 = CARTESIAN_POINT ( 'NONE',  ( -2.467881479971292258, -8.804721359397014169, -12.36426617047028387 ) ) ;
#6515 = VECTOR ( 'NONE', #21747, 1000.000000000000000 ) ;
#6516 = DIRECTION ( 'NONE',  ( -1.000000000000000000, -0.000000000000000000, -0.000000000000000000 ) ) ;
#6517 = ORIENTED_EDGE ( 'NONE', *, *, #13555, .T. ) ;
#6518 = DIRECTION ( 'NONE',  ( -1.000000000000000000, 0.000000000000000000, 0.000000000000000000 ) ) ;
#6519 = EDGE_CURVE ( 'NONE', #13407, #15351, #12944, .T. ) ;
#6520 = ORIENTED_EDGE ( 'NONE', *, *, #11367, .T. ) ;
#6521 = DIRECTION ( 'NONE',  ( 1.000000000000000000, 0.000000000000000000, 0.000000000000000000 ) ) ;
#6522 = PRODUCT_DEFINITION_SHAPE ( 'NONE', 'NONE',  #13308 ) ;
#6523 = DIRECTION ( 'NONE',  ( 1.000000000000000000, 0.000000000000000000, 0.000000000000000000 ) ) ;
#6524 = LINE ( 'NONE', #12094, #16879 ) ;
#6525 = DIRECTION ( 'NONE',  ( 1.000000000000000000, 0.000000000000000000, 0.000000000000000000 ) ) ;
#6526 = EDGE_LOOP ( 'NONE', ( #4621, #6804, #24017, #3769 ) ) ;
#6527 = APPLICATION_CONTEXT ( 'automotive_design' ) ;
#6528 = FACE_OUTER_BOUND ( 'NONE', #13209, .T. ) ;
#6529 = CARTESIAN_POINT ( 'NONE',  ( -28.99999999999999645, 29.50000000000000711, 0.000000000000000000 ) ) ;
#6530 = EDGE_CURVE ( 'NONE', #3165, #8486, #11699, .T. ) ;
#6531 = DIRECTION ( 'NONE',  ( -1.000000000000000000, 0.000000000000000000, 0.000000000000000000 ) ) ;
#6532 = VERTEX_POINT ( 'NONE', #4420 ) ;
#6533 = EDGE_CURVE ( 'NONE', #10574, #5706, #11834, .T. ) ;
#6534 = CARTESIAN_POINT ( 'NONE',  ( -9.499999999999790390, -3.086737114213257804, 5.159589141758141650 ) ) ;
#6535 = EDGE_LOOP ( 'NONE', ( #19906, #24062, #20460, #14143 ) ) ;
#6536 = ORIENTED_EDGE ( 'NONE', *, *, #1160, .F. ) ;
#6537 = ORIENTED_EDGE ( 'NONE', *, *, #23603, .F. ) ;
#6538 = ORIENTED_EDGE ( 'NONE', *, *, #19524, .T. ) ;
#6539 = CARTESIAN_POINT ( 'NONE',  ( 41.00000000000000000, 26.23076770084981746, 12.00000000000000000 ) ) ;
#6540 = DIRECTION ( 'NONE',  ( 0.000000000000000000, 0.000000000000000000, -1.000000000000000000 ) ) ;
#6541 = DIRECTION ( 'NONE',  ( 3.469446951953610639E-15, -1.000000000000000000, 0.000000000000000000 ) ) ;
#6542 = CARTESIAN_POINT ( 'NONE',  ( -9.500000000000000000, 0.000000000000000000, 12.50000000000000000 ) ) ;
#6543 = ORIENTED_EDGE ( 'NONE', *, *, #6041, .T. ) ;
#6544 = CARTESIAN_POINT ( 'NONE',  ( -16.36153765883235423, -6.593687918952691795, 6.842832175870698919 ) ) ;
#6545 = DIRECTION ( 'NONE',  ( 0.000000000000000000, 0.000000000000000000, 1.000000000000000000 ) ) ;
#6546 = LINE ( 'NONE', #8586, #17505 ) ;
#6547 = VERTEX_POINT ( 'NONE', #10116 ) ;
#6548 = CARTESIAN_POINT ( 'NONE',  ( 84.18181818181818699, 4.172000000000015696, 0.000000000000000000 ) ) ;
#6549 = CARTESIAN_POINT ( 'NONE',  ( -9.500000000000000000, -6.482511860946779655E-13, 7.059589141758143782 ) ) ;
#6550 = CARTESIAN_POINT ( 'NONE',  ( 2.935661446562616295, -9.035036904803758873, 6.806742014460233747 ) ) ;
#6551 = DIRECTION ( 'NONE',  ( -1.000000000000000000, 0.000000000000000000, 0.000000000000000000 ) ) ;
#6552 = CARTESIAN_POINT ( 'NONE',  ( 30.44534269664590909, -40.40463133211080304, 27.00000000000000000 ) ) ;
#6553 = CIRCLE ( 'NONE', #18233, 5.000000000000000888 ) ;
#6554 = DIRECTION ( 'NONE',  ( -0.7071067811865443531, 0.000000000000000000, -0.7071067811865506814 ) ) ;
#6555 = AXIS2_PLACEMENT_3D ( 'NONE', #11611, #6391, #2238 ) ;
#6556 = CARTESIAN_POINT ( 'NONE',  ( 14.98952570844869747, 0.6468970097546595799, 9.483487670324109331 ) ) ;
#6557 = CARTESIAN_POINT ( 'NONE',  ( 8.680847955710813579, 2.820578480814259326, -4.733165578109188587 ) ) ;
#6558 = EDGE_CURVE ( 'NONE', #5096, #13543, #13602, .T. ) ;
#6559 = DIRECTION ( 'NONE',  ( -0.000000000000000000, 1.000000000000000000, -0.000000000000000000 ) ) ;
#6560 = ORIENTED_EDGE ( 'NONE', *, *, #9291, .F. ) ;
#6561 = ORIENTED_EDGE ( 'NONE', *, *, #9676, .F. ) ;
#6562 = CARTESIAN_POINT ( 'NONE',  ( 2.682529543899157876, 8.255977015246598327, -11.03316557810918752 ) ) ;
#6563 = CARTESIAN_POINT ( 'NONE',  ( 8.680847955710813579, 2.820578480814259326, 8.733165578109185034 ) ) ;
#6564 = ORIENTED_EDGE ( 'NONE', *, *, #1411, .T. ) ;
#6565 =( NAMED_UNIT ( * ) SI_UNIT ( $, .STERADIAN. ) SOLID_ANGLE_UNIT ( ) );
#6566 = DIRECTION ( 'NONE',  ( -0.000000000000000000, -0.000000000000000000, -1.000000000000000000 ) ) ;
#6567 = EDGE_LOOP ( 'NONE', ( #17799, #9493, #11772, #7121 ) ) ;
#6568 = DIRECTION ( 'NONE',  ( 0.000000000000000000, -0.000000000000000000, -1.000000000000000000 ) ) ;
#6569 = CARTESIAN_POINT ( 'NONE',  ( 0.000000000000000000, 0.000000000000000000, 15.50000000000000000 ) ) ;
#6570 = CIRCLE ( 'NONE', #9648, 5.100000000000000533 ) ;
#6571 = CIRCLE ( 'NONE', #5028, 8.999999999999994671 ) ;
#6572 = CARTESIAN_POINT ( 'NONE',  ( 40.23082370883260239, 29.49999999999999645, -1.500000000000000000 ) ) ;
#6573 = CARTESIAN_POINT ( 'NONE',  ( -34.00000000000000000, -3.851859888774471706E-31, 11.00000000000000000 ) ) ;
#6574 = CARTESIAN_POINT ( 'NONE',  ( 23.00000000000000000, 12.00453763395396756, -7.608955687739546114 ) ) ;
#6575 = ORIENTED_EDGE ( 'NONE', *, *, #5440, .T. ) ;
#6576 = ADVANCED_FACE ( 'NONE', ( #7796 ), #20759, .F. ) ;
#6577 = LINE ( 'NONE', #14354, #23095 ) ;
#6578 = EDGE_CURVE ( 'NONE', #15489, #9530, #15376, .T. ) ;
#6579 = CARTESIAN_POINT ( 'NONE',  ( -28.99999999999999645, 29.50000000000000000, 27.00000000000000000 ) ) ;
#6580 = VECTOR ( 'NONE', #11708, 1000.000000000000000 ) ;
#6581 = ORIENTED_EDGE ( 'NONE', *, *, #14880, .F. ) ;
#6582 = CARTESIAN_POINT ( 'NONE',  ( 60.32931906745326245, 7.420530141404717394E-15, 0.000000000000000000 ) ) ;
#6583 = CARTESIAN_POINT ( 'NONE',  ( -42.00000000000000000, 0.000000000000000000, 12.00000000000000000 ) ) ;
#6584 = CARTESIAN_POINT ( 'NONE',  ( -30.44534269664590553, -40.40463133211081015, 12.00000000000000000 ) ) ;
#6585 = EDGE_CURVE ( 'NONE', #13405, #2012, #6361, .T. ) ;
#6586 = CYLINDRICAL_SURFACE ( 'NONE', #13809, 20.85000000000000142 ) ;
#6587 = ORIENTED_EDGE ( 'NONE', *, *, #5507, .T. ) ;
#6588 = B_SPLINE_CURVE_WITH_KNOTS ( 'NONE', 3,
 ( #281, #22589, #2588, #640, #13296, #9639, #11698, #13179, #2450, #16834, #4049, #15235, #22487, #17085, #20638, #388, #5763, #20893 ),
 .UNSPECIFIED., .F., .F.,
 ( 4, 2, 2, 2, 2, 2, 2, 2, 4 ),
 ( 0.004724984058646233484, 0.005314812857951324923, 0.005904641657256416362, 0.006494470456561507801, 0.007084299255866599240, 0.007674128055171690679, 0.008263956854476782118, 0.008853785653781873557, 0.009443614453086964997 ),
 .UNSPECIFIED. ) ;
#6589 = CARTESIAN_POINT ( 'NONE',  ( -7.685661446561619314, -5.583959896779019161, -12.40674201446023339 ) ) ;
#6590 = ORIENTED_EDGE ( 'NONE', *, *, #18442, .F. ) ;
#6591 = ORIENTED_EDGE ( 'NONE', *, *, #4628, .F. ) ;
#6592 = CARTESIAN_POINT ( 'NONE',  ( 9.500000000000000000, 6.470877716354879437E-13, 4.059589141758143782 ) ) ;
#6593 = CARTESIAN_POINT ( 'NONE',  ( 7.937578510445243651, -3.514536757623948127, -12.49999999999998046 ) ) ;
#6594 = ORIENTED_EDGE ( 'NONE', *, *, #20077, .T. ) ;
#6595 = FACE_OUTER_BOUND ( 'NONE', #2833, .T. ) ;
#6596 = DIRECTION ( 'NONE',  ( 0.000000000000000000, -1.000000000000000000, 0.000000000000000000 ) ) ;
#6597 = FACE_OUTER_BOUND ( 'NONE', #20772, .T. ) ;
#6598 = CARTESIAN_POINT ( 'NONE',  ( 35.99999999999999289, 50.99999999999999289, 0.5000000000000004441 ) ) ;
#6599 = DIRECTION ( 'NONE',  ( 0.000000000000000000, -1.000000000000000000, 0.000000000000000000 ) ) ;
#6600 = EDGE_LOOP ( 'NONE', ( #4629, #12273, #21022, #14372 ) ) ;
#6601 = DIRECTION ( 'NONE',  ( 0.000000000000000000, 0.000000000000000000, -1.000000000000000000 ) ) ;
#6602 = ADVANCED_FACE ( 'NONE', ( #21254 ), #22712, .T. ) ;
#6603 = EDGE_CURVE ( 'NONE', #22613, #8771, #11769, .T. ) ;
#6604 = ORIENTED_EDGE ( 'NONE', *, *, #930, .T. ) ;
#6605 = CARTESIAN_POINT ( 'NONE',  ( 67.60204634018053582, 7.420530141404717394E-15, 0.000000000000000000 ) ) ;
#6606 = CARTESIAN_POINT ( 'NONE',  ( 9.500000000000000000, 1.163414459189985485E-15, 12.50000000000000000 ) ) ;
#6607 = DIRECTION ( 'NONE',  ( 1.000000000000000000, 0.000000000000000000, 0.000000000000000000 ) ) ;
#6608 = CARTESIAN_POINT ( 'NONE',  ( 86.51113724927145654, 5.000000000000007105, 6.123233995736765296E-16 ) ) ;
#6609 = DIRECTION ( 'NONE',  ( -0.8571673007021116675, 1.049727191138617833E-16, 0.5150380749100552658 ) ) ;
#6610 = ORIENTED_EDGE ( 'NONE', *, *, #18248, .F. ) ;
#6611 = DIRECTION ( 'NONE',  ( 0.000000000000000000, 0.5406408174555987767, -0.8412535328311804284 ) ) ;
#6612 = EDGE_LOOP ( 'NONE', ( #3939, #77, #5849 ) ) ;
#6613 = CARTESIAN_POINT ( 'NONE',  ( 89.12522638709219791, 6.123233995736675563E-16, -5.000000000000007994 ) ) ;
#6614 = ORIENTED_EDGE ( 'NONE', *, *, #3572, .T. ) ;
#6615 = VECTOR ( 'NONE', #21113, 1000.000000000000000 ) ;
#6616 = LINE ( 'NONE', #19907, #22693 ) ;
#6617 = FACE_OUTER_BOUND ( 'NONE', #23425, .T. ) ;
#6618 = B_SPLINE_CURVE_WITH_KNOTS ( 'NONE', 3,
 ( #6668, #3016, #18005, #19483, #17895, #1183, #23639, #13874, #2884, #19848, #3119, #4610, #8596, #6912, #16043, #10542, #23505, #10175, #15816, #11899, #8723, #6786, #14216, #16175, #14332, #17632, #23148, #4490, #19372, #12012, #3362, #1888, #3239, #20202, #3588, #1433 ),
 .UNSPECIFIED., .F., .F.,
 ( 4, 2, 2, 2, 2, 2, 2, 2, 2, 2, 2, 2, 2, 2, 2, 2, 2, 4 ),
 ( 3.004629197474318463E-18, 0.002901772246161926725, 0.003627215307702404828, 0.004352658369242881631, 0.005803544492323830899, 0.006528987553864306834, 0.007254430615404782769, 0.008705316738485735506, 0.01015620286156668911, 0.01160708898464764098, 0.01305797510772859632, 0.01450886123080954992, 0.01595974735389050353, 0.01741063347697145713, 0.01886151960005241074, 0.02031240572313336781, 0.02176329184621432142, 0.02321417796929527502 ),
 .UNSPECIFIED. ) ;
#6619 = DIRECTION ( 'NONE',  ( 1.000000000000000000, 0.000000000000000000, 0.000000000000000000 ) ) ;
#6620 = ORIENTED_EDGE ( 'NONE', *, *, #10122, .F. ) ;
#6621 = ADVANCED_FACE ( 'NONE', ( #2334 ), #11957, .T. ) ;
#6622 = ORIENTED_EDGE ( 'NONE', *, *, #15548, .F. ) ;
#6623 = CONTEXT_DEPENDENT_SHAPE_REPRESENTATION ( #19644, #15094 ) ;
#6624 = ORIENTED_EDGE ( 'NONE', *, *, #19495, .T. ) ;
#6625 = DIRECTION ( 'NONE',  ( 0.000000000000000000, 0.000000000000000000, 1.000000000000000000 ) ) ;
#6626 = AXIS2_PLACEMENT_3D ( 'NONE', #1547, #3374, #1314 ) ;
#6627 = ORIENTED_EDGE ( 'NONE', *, *, #1321, .F. ) ;
#6628 = CARTESIAN_POINT ( 'NONE',  ( 23.97500000000000497, -29.50000000000000000, -3.000000000000000000 ) ) ;
#6629 = VECTOR ( 'NONE', #1180, 1000.000000000000000 ) ;
#6630 = EDGE_CURVE ( 'NONE', #3540, #13580, #4297, .T. ) ;
#6631 = EDGE_CURVE ( 'NONE', #14710, #9726, #5176, .T. ) ;
#6632 = DIRECTION ( 'NONE',  ( 1.000000000000000000, 0.000000000000000000, 0.000000000000000000 ) ) ;
#6633 = VERTEX_POINT ( 'NONE', #22963 ) ;
#6634 = DIRECTION ( 'NONE',  ( 0.8757121056631640421, 0.4828336235133042775, -0.000000000000000000 ) ) ;
#6635 = ORIENTED_EDGE ( 'NONE', *, *, #1717, .F. ) ;
#6636 = CARTESIAN_POINT ( 'NONE',  ( 76.03431729618309021, 7.562528597612068045E-15, 0.000000000000000000 ) ) ;
#6637 = CARTESIAN_POINT ( 'NONE',  ( 0.000000000000000000, 0.000000000000000000, 0.4999999999999995559 ) ) ;
#6638 = CARTESIAN_POINT ( 'NONE',  ( -41.73082370883257397, -27.62204025492845361, -1.500000000000000000 ) ) ;
#6639 = CARTESIAN_POINT ( 'NONE',  ( 39.00000000000000000, 0.000000000000000000, 11.00000000000000000 ) ) ;
#6640 = CARTESIAN_POINT ( 'NONE',  ( 35.99999999999992184, 59.99999999999998579, 12.50000000000000000 ) ) ;
#6641 = ORIENTED_EDGE ( 'NONE', *, *, #10765, .T. ) ;
#6642 = DIRECTION ( 'NONE',  ( 1.000000000000000000, 0.000000000000000000, 0.000000000000000000 ) ) ;
#6643 = FACE_OUTER_BOUND ( 'NONE', #17008, .T. ) ;
#6644 = CARTESIAN_POINT ( 'NONE',  ( 5.000000000000000000, -2.342598717236905603, 4.057500000000010765 ) ) ;
#6645 = CARTESIAN_POINT ( 'NONE',  ( -6.822232771736903637E-13, 9.988891130263535700, 4.559589141758142894 ) ) ;
#6646 = VECTOR ( 'NONE', #16342, 1000.000000000000000 ) ;
#6647 = VERTEX_POINT ( 'NONE', #2219 ) ;
#6648 = EDGE_CURVE ( 'NONE', #13339, #12632, #8666, .T. ) ;
#6649 = ORIENTED_EDGE ( 'NONE', *, *, #3122, .T. ) ;
#6650 = ORIENTED_EDGE ( 'NONE', *, *, #2767, .F. ) ;
#6651 = DIRECTION ( 'NONE',  ( 0.7071067811865443531, 8.659560562354894648E-17, -0.7071067811865506814 ) ) ;
#6652 = CARTESIAN_POINT ( 'NONE',  ( -2.935661446562617183, 9.035036904803758873, 7.806742014460233747 ) ) ;
#6653 = FACE_OUTER_BOUND ( 'NONE', #20812, .T. ) ;
#6654 = ORIENTED_EDGE ( 'NONE', *, *, #11774, .F. ) ;
#6655 = DIRECTION ( 'NONE',  ( -0.000000000000000000, 1.000000000000000000, -0.000000000000000000 ) ) ;
#6656 = FACE_OUTER_BOUND ( 'NONE', #9787, .T. ) ;
#6657 = EDGE_CURVE ( 'NONE', #20027, #18466, #389, .T. ) ;
#6658 = ADVANCED_FACE ( 'NONE', ( #17337 ), #641, .T. ) ;
#6659 = CARTESIAN_POINT ( 'NONE',  ( 41.73082370883260239, 29.49999999999999645, -1.500000000000000000 ) ) ;
#6660 = ORIENTED_EDGE ( 'NONE', *, *, #9989, .T. ) ;
#6661 = DIRECTION ( 'NONE',  ( 1.000000000000000000, 0.000000000000000000, 0.000000000000000000 ) ) ;
#6662 = CARTESIAN_POINT ( 'NONE',  ( 78.36363636363637397, -4.172000000000000597, 5.616230220889771312E-16 ) ) ;
#6663 = CARTESIAN_POINT ( 'NONE',  ( -5.871322893124554021, 8.081182679343978492, 5.906742014460233392 ) ) ;
#6664 = CIRCLE ( 'NONE', #3535, 0.2999999999999999334 ) ;
#6665 = CARTESIAN_POINT ( 'NONE',  ( -40.23082370883260239, 27.62204025492846071, -3.000000000000000000 ) ) ;
#6666 = DIRECTION ( 'NONE',  ( -1.000000000000000000, 0.000000000000000000, 0.000000000000000000 ) ) ;
#6667 = CARTESIAN_POINT ( 'NONE',  ( 0.000000000000000000, -45.00000000000000000, 3.000000000000002665 ) ) ;
#6668 = CARTESIAN_POINT ( 'NONE',  ( 14.51962751333974211, -3.765689428759034563, -8.721787840009190163 ) ) ;
#6669 = DIRECTION ( 'NONE',  ( -0.000000000000000000, 0.000000000000000000, 1.000000000000000000 ) ) ;
#6670 = CARTESIAN_POINT ( 'NONE',  ( 2.682529543899157876, 8.255977015246598327, -11.03316557810918752 ) ) ;
#6671 = ORIENTED_EDGE ( 'NONE', *, *, #21598, .T. ) ;
#6672 = DIRECTION ( 'NONE',  ( 0.000000000000000000, 0.000000000000000000, 1.000000000000000000 ) ) ;
#6673 = ORIENTED_EDGE ( 'NONE', *, *, #22096, .F. ) ;
#6674 = LINE ( 'NONE', #14106, #6580 ) ;
#6675 = VERTEX_POINT ( 'NONE', #20233 ) ;
#6676 = DIRECTION ( 'NONE',  ( -8.408933298497765619E-17, -2.748362728120539922E-17, -1.000000000000000000 ) ) ;
#6677 = EDGE_CURVE ( 'NONE', #1409, #2972, #13934, .T. ) ;
#6678 = DIRECTION ( 'NONE',  ( 1.000000000000000000, 0.000000000000000000, -0.000000000000000000 ) ) ;
#6679 = AXIS2_PLACEMENT_3D ( 'NONE', #10180, #17640, #13994 ) ;
#6680 = VERTEX_POINT ( 'NONE', #18042 ) ;
#6681 = ORIENTED_EDGE ( 'NONE', *, *, #1025, .F. ) ;
#6682 = FACE_OUTER_BOUND ( 'NONE', #22147, .T. ) ;
#6683 = CARTESIAN_POINT ( 'NONE',  ( -5.871322893124554021, 8.081182679343978492, -4.759589141758144848 ) ) ;
#6684 = UNCERTAINTY_MEASURE_WITH_UNIT (LENGTH_MEASURE( 1.000000000000000082E-05 ), #10220, 'distance_accuracy_value', 'NONE');
#6685 = CIRCLE ( 'NONE', #21882, 4.172000000000008590 ) ;
#6686 = CARTESIAN_POINT ( 'NONE',  ( -2.384317694982191593, 8.679161036964110565, 100.8311869460038253 ) ) ;
#6687 = CARTESIAN_POINT ( 'NONE',  ( 8.417661073264101290, -2.391602252564205777, 12.49999999999999822 ) ) ;
#6688 = CYLINDRICAL_SURFACE ( 'NONE', #12384, 6.050000000006050982 ) ;
#6689 = EDGE_CURVE ( 'NONE', #15771, #13623, #20344, .T. ) ;
#6690 = ORIENTED_EDGE ( 'NONE', *, *, #15703, .T. ) ;
#6691 = CARTESIAN_POINT ( 'NONE',  ( -12.50000000000000178, 1.672973214995343413E-15, 2.500000000000000000 ) ) ;
#6692 = DIRECTION ( 'NONE',  ( 1.000000000000000000, 6.485355633664481337E-14, 0.000000000000000000 ) ) ;
#6693 = CARTESIAN_POINT ( 'NONE',  ( 0.000000000000000000, 15.23000000000000220, 27.00000000000000000 ) ) ;
#6694 = ORIENTED_EDGE ( 'NONE', *, *, #17819, .F. ) ;
#6695 = DIRECTION ( 'NONE',  ( 0.000000000000000000, 0.8660254037844380415, -0.5000000000000011102 ) ) ;
#6696 = CARTESIAN_POINT ( 'NONE',  ( -30.68762588338046982, -45.64284848299540442, -1.500000000000000000 ) ) ;
#6697 = VECTOR ( 'NONE', #863, 1000.000000000000000 ) ;
#6698 = FACE_OUTER_BOUND ( 'NONE', #20074, .T. ) ;
#6699 = ORIENTED_EDGE ( 'NONE', *, *, #19778, .F. ) ;
#6700 = CIRCLE ( 'NONE', #4362, 5.000000000000007994 ) ;
#6701 = ORIENTED_EDGE ( 'NONE', *, *, #20818, .T. ) ;
#6702 = ORIENTED_EDGE ( 'NONE', *, *, #17522, .F. ) ;
#6703 = CARTESIAN_POINT ( 'NONE',  ( -5.871322893123450015, -8.081182679344781405, 7.359589141758143604 ) ) ;
#6704 = CARTESIAN_POINT ( 'NONE',  ( -6.822232771736903637E-13, 9.988891130263535700, 5.706742014460234103 ) ) ;
#6705 = VERTEX_POINT ( 'NONE', #10700 ) ;
#6706 = CARTESIAN_POINT ( 'NONE',  ( 35.99999999999999289, -51.00000000000000711, 0.000000000000000000 ) ) ;
#6707 = ADVANCED_FACE ( 'NONE', ( #10575 ), #19875, .T. ) ;
#6708 = DIRECTION ( 'NONE',  ( -1.000000000000000000, -1.224606353822377258E-16, -0.000000000000000000 ) ) ;
#6709 = CARTESIAN_POINT ( 'NONE',  ( -40.00000000000000000, 29.49999999999999645, 12.00000000000000000 ) ) ;
#6710 = AXIS2_PLACEMENT_3D ( 'NONE', #15709, #970, #19507 ) ;
#6711 = VECTOR ( 'NONE', #9349, 1000.000000000000000 ) ;
#6712 = SURFACE_STYLE_USAGE ( .BOTH. , #23682 ) ;
#6713 = ADVANCED_FACE ( 'NONE', ( #1339, #21942 ), #23773, .T. ) ;
#6714 = DIRECTION ( 'NONE',  ( -1.000000000000000000, 0.000000000000000000, 0.000000000000000000 ) ) ;
#6715 = EDGE_CURVE ( 'NONE', #11167, #16259, #22191, .T. ) ;
#6716 = LINE ( 'NONE', #21611, #21909 ) ;
#6717 = ORIENTED_EDGE ( 'NONE', *, *, #12208, .T. ) ;
#6718 = CARTESIAN_POINT ( 'NONE',  ( -23.89999999999999858, 29.50000000000000000, 27.00000000000000000 ) ) ;
#6719 = LINE ( 'NONE', #19670, #18368 ) ;
#6720 = CARTESIAN_POINT ( 'NONE',  ( -9.500000000000000000, -6.482511860946779655E-13, 11.05958914175814556 ) ) ;
#6721 = CARTESIAN_POINT ( 'NONE',  ( 8.932474687540359781, -3.867868693691564719, 11.92830913002138793 ) ) ;
#6722 = SURFACE_SIDE_STYLE ('',( #1365 ) ) ;
#6723 = DIRECTION ( 'NONE',  ( 0.000000000000000000, 0.9898214418809322401, 0.1423148382732887240 ) ) ;
#6724 = EDGE_LOOP ( 'NONE', ( #6794, #9643, #16529, #6462 ) ) ;
#6725 = LINE ( 'NONE', #15496, #5285 ) ;
#6726 = ORIENTED_EDGE ( 'NONE', *, *, #16437, .F. ) ;
#6727 = CARTESIAN_POINT ( 'NONE',  ( 42.00000000000000000, -25.93535998569253920, 27.00000000000000000 ) ) ;
#6728 = VERTEX_POINT ( 'NONE', #3510 ) ;
#6729 = CONICAL_SURFACE ( 'NONE', #7875, 9.000000000000001776, 0.7853981633974431720 ) ;
#6730 = CARTESIAN_POINT ( 'NONE',  ( 1.500000000000001332, 0.000000000000000000, 6.500000000000000888 ) ) ;
#6731 = CIRCLE ( 'NONE', #22319, 17.87500000001787726 ) ;
#6732 = AXIS2_PLACEMENT_3D ( 'NONE', #12412, #10343, #8517 ) ;
#6733 = EDGE_CURVE ( 'NONE', #20685, #11303, #20361, .T. ) ;
#6734 = DIRECTION ( 'NONE',  ( 0.000000000000000000, 0.5406408174555987767, -0.8412535328311804284 ) ) ;
#6735 = VECTOR ( 'NONE', #9881, 1000.000000000000000 ) ;
#6736 = CARTESIAN_POINT ( 'NONE',  ( 64.69295543108962931, 7.420530141404717394E-15, 0.000000000000000000 ) ) ;
#6737 = AXIS2_PLACEMENT_3D ( 'NONE', #6759, #12720, #16267 ) ;
#6738 = ADVANCED_FACE ( 'NONE', ( #6494 ), #23102, .T. ) ;
#6739 = CARTESIAN_POINT ( 'NONE',  ( -30.16774287754690675, -40.66994976491903913, -3.000000000000000000 ) ) ;
#6740 = CONICAL_SURFACE ( 'NONE', #21943, 1.000000000000000222, 0.7853981633974508325 ) ;
#6741 = EDGE_CURVE ( 'NONE', #14736, #4131, #3627, .T. ) ;
#6742 = ORIENTED_EDGE ( 'NONE', *, *, #894, .F. ) ;
#6743 = DIRECTION ( 'NONE',  ( 0.000000000000000000, -1.000000000000000000, 0.000000000000000000 ) ) ;
#6744 = CARTESIAN_POINT ( 'NONE',  ( -2.935661446561384391, -9.035036904804158553, -11.45958914175814414 ) ) ;
#6745 = CARTESIAN_POINT ( 'NONE',  ( 0.9902374497044862389, -9.042884052521602101, -12.43644623859449716 ) ) ;
#6746 = AXIS2_PLACEMENT_3D ( 'NONE', #3011, #21180, #23501 ) ;
#6747 = AXIS2_PLACEMENT_3D ( 'NONE', #1237, #24035, #14750 ) ;
#6748 = CIRCLE ( 'NONE', #19215, 11.24716442891539714 ) ;
#6749 = EDGE_LOOP ( 'NONE', ( #20130, #21633, #22566, #8140, #22562 ) ) ;
#6750 = DIRECTION ( 'NONE',  ( 0.000000000000000000, 0.000000000000000000, 1.000000000000000000 ) ) ;
#6751 = ORIENTED_EDGE ( 'NONE', *, *, #5515, .F. ) ;
#6752 = DIRECTION ( 'NONE',  ( -0.000000000000000000, 0.000000000000000000, 1.000000000000000000 ) ) ;
#6753 = CIRCLE ( 'NONE', #5559, 1.999999999999994449 ) ;
#6754 = DIRECTION ( 'NONE',  ( 0.000000000000000000, -0.000000000000000000, -1.000000000000000000 ) ) ;
#6755 = DIRECTION ( 'NONE',  ( -1.000000000000000000, 0.000000000000000000, 0.000000000000000000 ) ) ;
#6756 = DIRECTION ( 'NONE',  ( -1.000000000000000000, -0.000000000000000000, -0.000000000000000000 ) ) ;
#6757 = EDGE_LOOP ( 'NONE', ( #13745, #22610, #19654, #12735 ) ) ;
#6758 = DIRECTION ( 'NONE',  ( 1.000000000000000000, 0.000000000000000000, 0.000000000000000000 ) ) ;
#6759 = CARTESIAN_POINT ( 'NONE',  ( 76.32931906745326955, 7.420530141404717394E-15, 0.000000000000000000 ) ) ;
#6760 = CARTESIAN_POINT ( 'NONE',  ( 0.000000000000000000, 0.000000000000000000, 12.50000000000000000 ) ) ;
#6761 = CARTESIAN_POINT ( 'NONE',  ( 5.871322893124553133, -8.081182679343980269, 5.759589141758144848 ) ) ;
#6762 = CIRCLE ( 'NONE', #5187, 5.000000000000007994 ) ;
#6763 = EDGE_CURVE ( 'NONE', #12230, #4924, #23884, .T. ) ;
#6764 = VECTOR ( 'NONE', #13242, 1000.000000000000114 ) ;
#6765 = ORIENTED_EDGE ( 'NONE', *, *, #15502, .F. ) ;
#6766 = EDGE_CURVE ( 'NONE', #3765, #16958, #18169, .T. ) ;
#6767 = AXIS2_PLACEMENT_3D ( 'NONE', #6883, #21767, #14890 ) ;
#6768 = ORIENTED_EDGE ( 'NONE', *, *, #19577, .T. ) ;
#6769 = CONICAL_SURFACE ( 'NONE', #13762, 1.999999999999994449, 1.029744258676653201 ) ;
#6770 = AXIS2_PLACEMENT_3D ( 'NONE', #8711, #16160, #1418 ) ;
#6771 = AXIS2_PLACEMENT_3D ( 'NONE', #2221, #5511, #14892 ) ;
#6772 = ORIENTED_EDGE ( 'NONE', *, *, #9208, .F. ) ;
#6773 = VECTOR ( 'NONE', #309, 1000.000000000000000 ) ;
#6774 = DIRECTION ( 'NONE',  ( -0.000000000000000000, -0.000000000000000000, 1.000000000000000000 ) ) ;
#6775 = DIRECTION ( 'NONE',  ( -0.5735764363510519326, 0.8191520442889876907, 1.003171929053519816E-16 ) ) ;
#6776 = CARTESIAN_POINT ( 'NONE',  ( -17.06033556854818656, -8.068938288216807919, -5.036196554528634017 ) ) ;
#6777 = CARTESIAN_POINT ( 'NONE',  ( -31.74999999999995737, 6.123233995736767268E-16, -5.000000000000000888 ) ) ;
#6778 = ORIENTED_EDGE ( 'NONE', *, *, #19102, .F. ) ;
#6779 = CARTESIAN_POINT ( 'NONE',  ( 2.935661446562616295, -9.035036904803758873, -8.806742014460233747 ) ) ;
#6780 = LINE ( 'NONE', #16039, #5569 ) ;
#6781 = CARTESIAN_POINT ( 'NONE',  ( -2.935661446561384391, -9.035036904804158553, 6.606742014460233570 ) ) ;
#6782 = ORIENTED_EDGE ( 'NONE', *, *, #7326, .F. ) ;
#6783 = FACE_OUTER_BOUND ( 'NONE', #14250, .T. ) ;
#6784 = DIRECTION ( 'NONE',  ( 1.000000000000000000, 1.224606353822377258E-16, 0.000000000000000000 ) ) ;
#6785 = AXIS2_PLACEMENT_3D ( 'NONE', #2454, #17839, #8544 ) ;
#6786 = CARTESIAN_POINT ( 'NONE',  ( 17.52920230446416028, -9.315347328456290654, 1.925892650121551419 ) ) ;
#6787 = ADVANCED_FACE ( 'NONE', ( #19993 ), #5003, .T. ) ;
#6788 = CIRCLE ( 'NONE', #11810, 5.000000000000007994 ) ;
#6789 = CARTESIAN_POINT ( 'NONE',  ( 58.00000000000000000, 7.491529369508391930E-15, 0.000000000000000000 ) ) ;
#6790 = CIRCLE ( 'NONE', #5621, 4.499999999999997335 ) ;
#6791 = CYLINDRICAL_SURFACE ( 'NONE', #7903, 1.499999999999998002 ) ;
#6792 = VECTOR ( 'NONE', #4744, 1000.000000000000000 ) ;
#6793 = EDGE_CURVE ( 'NONE', #4778, #5547, #9814, .T. ) ;
#6794 = ORIENTED_EDGE ( 'NONE', *, *, #13419, .T. ) ;
#6795 = DIRECTION ( 'NONE',  ( -1.000000000000000000, -1.224606353822377258E-16, -0.000000000000000000 ) ) ;
#6796 = ORIENTED_EDGE ( 'NONE', *, *, #10988, .F. ) ;
#6797 = CARTESIAN_POINT ( 'NONE',  ( -8.680847955711200825, 2.820578480813073607, 5.533165578109187521 ) ) ;
#6798 = EDGE_CURVE ( 'NONE', #6647, #15351, #16469, .T. ) ;
#6799 = EDGE_CURVE ( 'NONE', #21725, #21270, #7170, .T. ) ;
#6800 = EDGE_CURVE ( 'NONE', #3619, #8857, #12202, .T. ) ;
#6801 = CARTESIAN_POINT ( 'NONE',  ( 693.7818939062881327, 843.4837211537981148, 1344.481724745927977 ) ) ;
#6802 = CARTESIAN_POINT ( 'NONE',  ( 0.000000000000000000, 0.000000000000000000, 27.00000000000000000 ) ) ;
#6803 = VERTEX_POINT ( 'NONE', #17568 ) ;
#6804 = ORIENTED_EDGE ( 'NONE', *, *, #13715, .F. ) ;
#6805 = DIRECTION ( 'NONE',  ( -1.000000000000000000, 0.000000000000000000, 0.000000000000000000 ) ) ;
#6806 = CARTESIAN_POINT ( 'NONE',  ( -9.500000000000211386, 3.086737114211961064, -8.959589141758140585 ) ) ;
#6807 = AXIS2_PLACEMENT_3D ( 'NONE', #17147, #446, #15444 ) ;
#6808 = CONICAL_SURFACE ( 'NONE', #4462, 10.50249999999999950, 0.7853981633974491672 ) ;
#6809 = CARTESIAN_POINT ( 'NONE',  ( 0.7803738342988795207, 8.968189405539467529, 101.9034025936691990 ) ) ;
#6810 = CARTESIAN_POINT ( 'NONE',  ( -34.00000000000000000, -3.851859888774471706E-31, 11.00000000000000000 ) ) ;
#6811 = LINE ( 'NONE', #14237, #7315 ) ;
#6812 = VECTOR ( 'NONE', #8811, 1000.000000000000000 ) ;
#6813 = ORIENTED_EDGE ( 'NONE', *, *, #6182, .T. ) ;
#6814 = CIRCLE ( 'NONE', #18120, 5.100000000000000533 ) ;
#6815 = DIRECTION ( 'NONE',  ( -1.000000000000000000, -0.000000000000000000, -0.000000000000000000 ) ) ;
#6816 = DIRECTION ( 'NONE',  ( 1.000000000000000000, 0.000000000000000000, 0.000000000000000000 ) ) ;
#6817 = DIRECTION ( 'NONE',  ( 0.000000000000000000, 0.000000000000000000, 1.000000000000000000 ) ) ;
#6818 = CARTESIAN_POINT ( 'NONE',  ( 84.18181818181818699, 7.491529369508391930E-15, 0.000000000000000000 ) ) ;
#6819 = EDGE_CURVE ( 'NONE', #16948, #2924, #8297, .T. ) ;
#6820 = CARTESIAN_POINT ( 'NONE',  ( 6.699999999999999289, 0.000000000000000000, 14.02592346138681201 ) ) ;
#6821 = ORIENTED_EDGE ( 'NONE', *, *, #11164, .F. ) ;
#6822 = CARTESIAN_POINT ( 'NONE',  ( -2.682529543899159208, -8.255977015246598327, -6.033165578109189298 ) ) ;
#6823 = VERTEX_POINT ( 'NONE', #21715 ) ;
#6824 = CIRCLE ( 'NONE', #17719, 5.000000000000004441 ) ;
#6825 = ORIENTED_EDGE ( 'NONE', *, *, #18150, .T. ) ;
#6826 = EDGE_CURVE ( 'NONE', #19949, #5846, #12962, .T. ) ;
#6827 = CARTESIAN_POINT ( 'NONE',  ( 9.500000000000209610, -3.086737114211962396, 13.10674201446023091 ) ) ;
#6828 = CARTESIAN_POINT ( 'NONE',  ( 6.809999908187194197E-13, -9.988891130263535700, 6.706742014460232326 ) ) ;
#6829 = ADVANCED_FACE ( 'NONE', ( #18749 ), #17659, .T. ) ;
#6830 = EDGE_CURVE ( 'NONE', #4702, #20316, #11165, .T. ) ;
#6831 = AXIS2_PLACEMENT_3D ( 'NONE', #9336, #9453, #5936 ) ;
#6832 = ORIENTED_EDGE ( 'NONE', *, *, #14383, .F. ) ;
#6833 = DIRECTION ( 'NONE',  ( 0.000000000000000000, 0.000000000000000000, 1.000000000000000000 ) ) ;
#6834 = VECTOR ( 'NONE', #16354, 1000.000000000000000 ) ;
#6835 = CARTESIAN_POINT ( 'NONE',  ( 30.44534269664590553, -40.40463133211081015, 0.000000000000000000 ) ) ;
#6836 = CARTESIAN_POINT ( 'NONE',  ( 6.809999908187194197E-13, -9.988891130263535700, -4.706742014460233214 ) ) ;
#6837 = CONICAL_SURFACE ( 'NONE', #21235, 4.172000000000008590, 0.9599310885968742602 ) ;
#6838 = COLOUR_RGB ( '',0.7921568627450980005, 0.8196078431372548767, 0.9333333333333333481 ) ;
#6839 = DIRECTION ( 'NONE',  ( 0.000000000000000000, 1.000000000000000000, 0.000000000000000000 ) ) ;
#6840 = CARTESIAN_POINT ( 'NONE',  ( 2.024999999999999911, -45.00000000000000000, -3.000000000000000000 ) ) ;
#6841 = DIRECTION ( 'NONE',  ( -1.000000000000000000, 0.000000000000000000, 0.000000000000000000 ) ) ;
#6842 = DIRECTION ( 'NONE',  ( 0.000000000000000000, 0.000000000000000000, -1.000000000000000000 ) ) ;
#6843 = EDGE_LOOP ( 'NONE', ( #23990, #4533, #2527, #6359, #16643, #20930 ) ) ;
#6844 =( REPRESENTATION_RELATIONSHIP ('NONE','NONE', #5350, #358 ) REPRESENTATION_RELATIONSHIP_WITH_TRANSFORMATION ( #4307 )SHAPE_REPRESENTATION_RELATIONSHIP( ) );
#6845 = CYLINDRICAL_SURFACE ( 'NONE', #5892, 49.99999999999999289 ) ;
#6846 = CARTESIAN_POINT ( 'NONE',  ( -2.935661446562617183, 9.035036904803758873, 10.65958914175814343 ) ) ;
#6848 = DIRECTION ( 'NONE',  ( 0.000000000000000000, 0.000000000000000000, -1.000000000000000000 ) ) ;
#6847 = VECTOR ( 'NONE', #22608, 1000.000000000000000 ) ;
#6849 = AXIS2_PLACEMENT_3D ( 'NONE', #5497, #3672, #10617 ) ;
#6850 = CARTESIAN_POINT ( 'NONE',  ( -1.999999999999994449, 45.00000000000000000, 23.99999999999999645 ) ) ;
#6851 = ORIENTED_EDGE ( 'NONE', *, *, #7719, .F. ) ;
#6852 = AXIS2_PLACEMENT_3D ( 'NONE', #4481, #17141, #15172 ) ;
#6853 = CARTESIAN_POINT ( 'NONE',  ( 29.00000000000000355, -29.50000000000000000, 12.50000000000000000 ) ) ;
#6854 = CIRCLE ( 'NONE', #13852, 4.999999999999997335 ) ;
#6855 = ORIENTED_EDGE ( 'NONE', *, *, #13570, .T. ) ;
#6856 = VERTEX_POINT ( 'NONE', #7858 ) ;
#6857 = DIRECTION ( 'NONE',  ( 0.000000000000000000, 0.000000000000000000, 1.000000000000000000 ) ) ;
#6858 = EDGE_CURVE ( 'NONE', #20829, #18077, #11537, .T. ) ;
#6859 = ORIENTED_EDGE ( 'NONE', *, *, #2126, .F. ) ;
#6860 = DIRECTION ( 'NONE',  ( -0.000000000000000000, -0.000000000000000000, -1.000000000000000000 ) ) ;
#6861 = DIRECTION ( 'NONE',  ( 1.000000000000000000, 0.000000000000000000, 0.000000000000000000 ) ) ;
#6862 = CARTESIAN_POINT ( 'NONE',  ( -1.749335460928132413, -9.337549220493531976, -3.500000000000076383 ) ) ;
#6863 = CARTESIAN_POINT ( 'NONE',  ( -40.66734255040736201, -26.56420859267092283, -3.000000000000000000 ) ) ;
#6864 = FACE_OUTER_BOUND ( 'NONE', #17311, .T. ) ;
#6865 = VECTOR ( 'NONE', #4807, 1000.000000000000000 ) ;
#6866 = AXIS2_PLACEMENT_3D ( 'NONE', #11414, #5594, #18889 ) ;
#6867 = ORIENTED_EDGE ( 'NONE', *, *, #2903, .F. ) ;
#6868 = DIRECTION ( 'NONE',  ( -1.000000000000000000, -1.224606353822377258E-16, -0.000000000000000000 ) ) ;
#6869 = AXIS2_PLACEMENT_3D ( 'NONE', #5114, #23433, #12534 ) ;
#6870 = CIRCLE ( 'NONE', #19736, 5.000000000000007994 ) ;
#6871 = CIRCLE ( 'NONE', #3363, 5.000000000000007994 ) ;
#6872 = CARTESIAN_POINT ( 'NONE',  ( -7.685661446561619314, -5.583959896779019161, -4.406742014460233392 ) ) ;
#6873 = ORIENTED_EDGE ( 'NONE', *, *, #16121, .F. ) ;
#6874 = VERTEX_POINT ( 'NONE', #20592 ) ;
#6875 = LINE ( 'NONE', #20171, #6812 ) ;
#6876 = EDGE_CURVE ( 'NONE', #19210, #10133, #3641, .T. ) ;
#6877 = DIRECTION ( 'NONE',  ( 0.000000000000000000, 0.000000000000000000, 1.000000000000000000 ) ) ;
#6878 = CARTESIAN_POINT ( 'NONE',  ( 84.76159002345582394, 7.562528597612068045E-15, 0.000000000000000000 ) ) ;
#6879 = EDGE_CURVE ( 'NONE', #1756, #18646, #7138, .T. ) ;
#6880 = ORIENTED_EDGE ( 'NONE', *, *, #5413, .T. ) ;
#6881 = VECTOR ( 'NONE', #16414, 1000.000000000000000 ) ;
#6882 = CARTESIAN_POINT ( 'NONE',  ( 0.6317332097104697564, -9.783628567664347742, -3.581108421866196156 ) ) ;
#6883 = CARTESIAN_POINT ( 'NONE',  ( 0.000000000000000000, 0.000000000000000000, 0.000000000000000000 ) ) ;
#6884 = ADVANCED_FACE ( 'NONE', ( #7395 ), #11403, .T. ) ;
#6885 = VECTOR ( 'NONE', #15457, 1000.000000000000000 ) ;
#6886 = CARTESIAN_POINT ( 'NONE',  ( -30.44534269664590553, 40.40463133211079594, 11.00000000000000000 ) ) ;
#6887 = VERTEX_POINT ( 'NONE', #3983 ) ;
#6888 = CARTESIAN_POINT ( 'NONE',  ( -6.153822176767817416E-13, 9.500000000000000000, -3.186529713919390439 ) ) ;
#6889 = EDGE_CURVE ( 'NONE', #14835, #13696, #3756, .T. ) ;
#6890 = CARTESIAN_POINT ( 'NONE',  ( 41.00000000000000000, 4.999999999999986677, 9.500000000000000000 ) ) ;
#6891 = CARTESIAN_POINT ( 'NONE',  ( 76.90909090909090651, -4.172000000000000597, 0.000000000000000000 ) ) ;
#6892 = CIRCLE ( 'NONE', #653, 0.7000000000000005107 ) ;
#6893 = CARTESIAN_POINT ( 'NONE',  ( -2.935661446561384391, -9.035036904804158553, 3.459589141758144137 ) ) ;
#6894 = VERTEX_POINT ( 'NONE', #18639 ) ;
#6895 = ORIENTED_EDGE ( 'NONE', *, *, #4493, .T. ) ;
#6896 = CARTESIAN_POINT ( 'NONE',  ( -23.97499999999999787, 29.50000000000000000, -3.000000000000000000 ) ) ;
#6897 = CIRCLE ( 'NONE', #20533, 17.87500000001787726 ) ;
#6898 = CARTESIAN_POINT ( 'NONE',  ( -9.500000000000000000, -6.482511860946779655E-13, 12.20674201446023410 ) ) ;
#6899 = DIRECTION ( 'NONE',  ( -0.000000000000000000, 0.000000000000000000, 1.000000000000000000 ) ) ;
#6900 = DIRECTION ( 'NONE',  ( -1.000000000000000000, 0.000000000000000000, 0.000000000000000000 ) ) ;
#6901 = CARTESIAN_POINT ( 'NONE',  ( -16.44572538483723534, -6.755397553796130161, 6.683320200552561374 ) ) ;
#6902 = EDGE_CURVE ( 'NONE', #14244, #13664, #526, .T. ) ;
#6903 = CARTESIAN_POINT ( 'NONE',  ( 58.57977184163763695, -5.000000000000000888, 6.123233995736776143E-16 ) ) ;
#6904 = ORIENTED_EDGE ( 'NONE', *, *, #15103, .F. ) ;
#6905 = FACE_OUTER_BOUND ( 'NONE', #514, .T. ) ;
#6906 = CYLINDRICAL_SURFACE ( 'NONE', #7496, 13.72592346138681130 ) ;
#6907 = CARTESIAN_POINT ( 'NONE',  ( 5.078177448618334644, 0.000000000000000000, 0.000000000000000000 ) ) ;
#6908 = EDGE_CURVE ( 'NONE', #16103, #10767, #9234, .T. ) ;
#6909 = ADVANCED_FACE ( 'NONE', ( #16915 ), #11045, .F. ) ;
#6910 = CARTESIAN_POINT ( 'NONE',  ( 0.000000000000000000, 0.000000000000000000, 27.00000000000000000 ) ) ;
#6911 = DIRECTION ( 'NONE',  ( 0.7071067811865439090, 8.659560562354888485E-17, -0.7071067811865512365 ) ) ;
#6912 = CARTESIAN_POINT ( 'NONE',  ( 17.32141611691247718, -8.728455122802969868, -3.780491077225275998 ) ) ;
#6913 = CARTESIAN_POINT ( 'NONE',  ( 42.00000000000000000, 5.999999999999986677, 12.00000000000000000 ) ) ;
#6914 = CARTESIAN_POINT ( 'NONE',  ( 6.222797240145152671E-13, -9.127583699786111282, -4.133165578109187166 ) ) ;
#6915 = VERTEX_POINT ( 'NONE', #22301 ) ;
#6916 = CARTESIAN_POINT ( 'NONE',  ( 2.682529543899157876, 8.255977015246598327, 11.03316557810918752 ) ) ;
#6917 = EDGE_LOOP ( 'NONE', ( #10351, #6113, #1839, #17343 ) ) ;
#6918 = PRODUCT_DEFINITION_SHAPE ( 'NONE', 'NONE',  #1431 ) ;
#6919 = DIRECTION ( 'NONE',  ( 5.551115123125782702E-17, 2.220446049250313081E-16, -1.000000000000000000 ) ) ;
#6920 = CARTESIAN_POINT ( 'NONE',  ( -21.84999999999999787, -16.67999999999984340, 12.00000000000000000 ) ) ;
#6921 = VERTEX_POINT ( 'NONE', #7750 ) ;
#6922 = VERTEX_POINT ( 'NONE', #9698 ) ;
#6923 = CYLINDRICAL_SURFACE ( 'NONE', #4098, 1.999999999999994449 ) ;
#6924 = CARTESIAN_POINT ( 'NONE',  ( -2.935661446562617183, 9.035036904803758873, -4.659589141758143427 ) ) ;
#6925 = PRODUCT_RELATED_PRODUCT_CATEGORY ( 'part', '', ( #10591 ) ) ;
#6926 = EDGE_CURVE ( 'NONE', #4459, #12416, #15310, .T. ) ;
#6927 = CARTESIAN_POINT ( 'NONE',  ( -2.693951614862269306, 8.587718935426160272, 100.3346014426491877 ) ) ;
#6928 = CARTESIAN_POINT ( 'NONE',  ( 41.51716637648670627, -25.94562225875360895, 12.00000000000000000 ) ) ;
#6929 = DIRECTION ( 'NONE',  ( -1.000000000000000000, 0.000000000000000000, 0.000000000000000000 ) ) ;
#6930 = DIRECTION ( 'NONE',  ( -0.000000000000000000, 0.000000000000000000, 1.000000000000000000 ) ) ;
#6931 = EDGE_CURVE ( 'NONE', #566, #22998, #8605, .T. ) ;
#6932 = FACE_OUTER_BOUND ( 'NONE', #22888, .T. ) ;
#6933 = EDGE_CURVE ( 'NONE', #12069, #3762, #2455, .T. ) ;
#6934 = ADVANCED_FACE ( 'NONE', ( #4857 ), #18252, .T. ) ;
#6935 = ORIENTED_EDGE ( 'NONE', *, *, #18496, .T. ) ;
#6936 = DIRECTION ( 'NONE',  ( -1.000000000000000000, 0.000000000000000000, 0.000000000000000000 ) ) ;
#6937 = ORIENTED_EDGE ( 'NONE', *, *, #15576, .T. ) ;
#6938 = LINE ( 'NONE', #2917, #11766 ) ;
#6939 = CARTESIAN_POINT ( 'NONE',  ( 72.54545454545454675, 4.172000000000015696, 5.109226446042767468E-16 ) ) ;
#6940 = SURFACE_SIDE_STYLE ('',( #20341 ) ) ;
#6941 = CARTESIAN_POINT ( 'NONE',  ( 2.454813078130514813E-15, -16.67999999999999972, 13.50000000000000178 ) ) ;
#6942 = VERTEX_POINT ( 'NONE', #16045 ) ;
#6943 = CARTESIAN_POINT ( 'NONE',  ( -37.00000000000000711, -29.49999999999999645, 11.50000000000000000 ) ) ;
#6944 = FACE_OUTER_BOUND ( 'NONE', #22022, .T. ) ;
#6945 = ORIENTED_EDGE ( 'NONE', *, *, #869, .F. ) ;
#6946 = ORIENTED_EDGE ( 'NONE', *, *, #20515, .F. ) ;
#6947 = CARTESIAN_POINT ( 'NONE',  ( -7.685661446562381371, 5.583959896777970222, 4.859589141758143604 ) ) ;
#6948 = CARTESIAN_POINT ( 'NONE',  ( -7.685661446562381371, 5.583959896777970222, 10.00674201446023481 ) ) ;
#6949 = DIRECTION ( 'NONE',  ( 0.000000000000000000, 1.000000000000000000, 0.000000000000000000 ) ) ;
#6950 = CONICAL_SURFACE ( 'NONE', #20580, 5.000000000000007994, 0.9599310885968855844 ) ;
#6951 = ORIENTED_EDGE ( 'NONE', *, *, #16151, .F. ) ;
#6952 = DIRECTION ( 'NONE',  ( -0.000000000000000000, 0.000000000000000000, -1.000000000000000000 ) ) ;
#6953 = CARTESIAN_POINT ( 'NONE',  ( -30.68762588338048403, 45.64284848299540442, -1.500000000000000000 ) ) ;
#6954 = CARTESIAN_POINT ( 'NONE',  ( 65.27272727272728048, 4.172000000000015696, 0.000000000000000000 ) ) ;
#6955 = ADVANCED_FACE ( 'NONE', ( #7016 ), #1186, .F. ) ;
#6956 = CYLINDRICAL_SURFACE ( 'NONE', #3649, 5.000000000000000888 ) ;
#6957 = CARTESIAN_POINT ( 'NONE',  ( -1.000000000000000222, 1.224646799147353454E-16, 0.2999999999999990452 ) ) ;
#6958 = ORIENTED_EDGE ( 'NONE', *, *, #23438, .T. ) ;
#6959 = ADVANCED_FACE ( 'NONE', ( #9075 ), #6791, .F. ) ;
#6960 = ADVANCED_FACE ( 'NONE', ( #14220 ), #6769, .F. ) ;
#6961 = EDGE_LOOP ( 'NONE', ( #10325, #1278, #15792, #19583, #13626, #2626, #611, #8373, #4980, #8069, #2137, #1972, #16383, #14943, #10292, #23116, #11544, #3087, #11073, #4585, #9358, #1100, #6604, #5226, #7334, #16981, #14809, #11077, #1466, #9183, #19231, #2737, #22581, #5130, #19920, #19222, #9723, #21714, #7125, #21223, #22819, #10507, #2288, #12932, #22809, #8936, #1191, #22734 ) ) ;
#6962 = FACE_BOUND ( 'NONE', #13085, .T. ) ;
#6963 = CARTESIAN_POINT ( 'NONE',  ( -1.999999999999994449, 45.00000000000000000, -27.00000000000000000 ) ) ;
#6964 = CARTESIAN_POINT ( 'NONE',  ( -2.166966487431423616, 9.254762091183735606, -3.500972724454019858 ) ) ;
#6965 = CARTESIAN_POINT ( 'NONE',  ( -45.00000000000000000, -50.99999999999993605, 12.50000000000000000 ) ) ;
#6966 =( GEOMETRIC_REPRESENTATION_CONTEXT ( 3 ) GLOBAL_UNCERTAINTY_ASSIGNED_CONTEXT ( ( #3033 ) ) GLOBAL_UNIT_ASSIGNED_CONTEXT ( ( #751, #5993, #637 ) ) REPRESENTATION_CONTEXT ( 'NONE', 'WORKASPACE' ) );
#6967 = DIRECTION ( 'NONE',  ( -0.000000000000000000, -0.000000000000000000, -1.000000000000000000 ) ) ;
#6968 = CARTESIAN_POINT ( 'NONE',  ( -7.022953521754877748, -5.102474405760673015, -9.833165578109188232 ) ) ;
#6969 = CARTESIAN_POINT ( 'NONE',  ( 28.27483331787887622, 41.23752903419610050, -27.00000000000000000 ) ) ;
#6970 = ORIENTED_EDGE ( 'NONE', *, *, #19932, .T. ) ;
#6971 = CARTESIAN_POINT ( 'NONE',  ( -34.00000000000000000, -3.851859888774471706E-31, 9.500000000000000000 ) ) ;
#6972 = ORIENTED_EDGE ( 'NONE', *, *, #12992, .F. ) ;
#6973 = CARTESIAN_POINT ( 'NONE',  ( -8.680847955710813579, -2.820578480814257549, 3.733165578109188587 ) ) ;
#6974 = ORIENTED_EDGE ( 'NONE', *, *, #13645, .T. ) ;
#6975 = CARTESIAN_POINT ( 'NONE',  ( 81.85249911436491743, -5.000000000000000888, 6.123233995736776143E-16 ) ) ;
#6976 = DIRECTION ( 'NONE',  ( -1.000000000000000000, -1.224606353822377258E-16, -0.000000000000000000 ) ) ;
#6977 = CARTESIAN_POINT ( 'NONE',  ( -9.000000000000000000, 0.000000000000000000, 51.99999999999998579 ) ) ;
#6978 = APPLICATION_CONTEXT ( 'automotive_design' ) ;
#6979 = CARTESIAN_POINT ( 'NONE',  ( 0.000000000000000000, 0.000000000000000000, 0.000000000000000000 ) ) ;
#6980 = CARTESIAN_POINT ( 'NONE',  ( -5.871322893124554021, 8.081182679343978492, -3.906742014460231616 ) ) ;
#6981 = VERTEX_POINT ( 'NONE', #12495 ) ;
#6982 = CARTESIAN_POINT ( 'NONE',  ( 0.000000000000000000, 45.00000000000000000, -26.97499999999999432 ) ) ;
#6983 = ADVANCED_FACE ( 'NONE', ( #12387 ), #23849, .T. ) ;
#6984 = EDGE_CURVE ( 'NONE', #16942, #16055, #5192, .T. ) ;
#6985 = ORIENTED_EDGE ( 'NONE', *, *, #18967, .T. ) ;
#6986 = CYLINDRICAL_SURFACE ( 'NONE', #10593, 4.999999999999997335 ) ;
#6987 = LINE ( 'NONE', #16143, #22360 ) ;
#6988 = ORIENTED_EDGE ( 'NONE', *, *, #7892, .F. ) ;
#6989 = DIRECTION ( 'NONE',  ( 0.000000000000000000, -1.000000000000000000, 0.000000000000000000 ) ) ;
#6990 = DIRECTION ( 'NONE',  ( -0.000000000000000000, -0.000000000000000000, 1.000000000000000000 ) ) ;
#6991 = FACE_BOUND ( 'NONE', #19617, .T. ) ;
#6992 = CARTESIAN_POINT ( 'NONE',  ( 7.685661446562381371, -5.583959896777971110, 3.859589141758143604 ) ) ;
#6993 = EDGE_LOOP ( 'NONE', ( #481, #2561, #11154, #4480 ) ) ;
#6994 = ADVANCED_FACE ( 'NONE', ( #10544 ), #22345, .T. ) ;
#6995 = EDGE_LOOP ( 'NONE', ( #13880, #18809, #23658, #10355, #2821 ) ) ;
#6996 = AXIS2_PLACEMENT_3D ( 'NONE', #9514, #6231, #21001 ) ;
#6997 = ADVANCED_FACE ( 'NONE', ( #12745 ), #20206, .F. ) ;
#6998 = ORIENTED_EDGE ( 'NONE', *, *, #22221, .T. ) ;
#6999 = CARTESIAN_POINT ( 'NONE',  ( 0.000000000000000000, 15.03999999999999737, 0.000000000000000000 ) ) ;
#7000 = DIRECTION ( 'NONE',  ( -1.000000000000000000, -0.000000000000000000, 0.000000000000000000 ) ) ;
#7001 = DIRECTION ( 'NONE',  ( 0.000000000000000000, -0.9096319953545137782, -0.4154150130018967602 ) ) ;
#7002 = EDGE_LOOP ( 'NONE', ( #1548, #19884, #20583, #9816 ) ) ;
#7003 = ORIENTED_EDGE ( 'NONE', *, *, #11746, .T. ) ;
#7004 = EDGE_CURVE ( 'NONE', #23803, #16388, #16094, .T. ) ;
#7005 = EDGE_CURVE ( 'NONE', #2972, #23101, #8727, .T. ) ;
#7006 = CARTESIAN_POINT ( 'NONE',  ( 10.83999999999999986, -14.99147757894464306, 15.50000000000000000 ) ) ;
#7007 = ORIENTED_EDGE ( 'NONE', *, *, #11612, .T. ) ;
#7008 = DIRECTION ( 'NONE',  ( 1.000000000000000000, 0.000000000000000000, 0.000000000000000000 ) ) ;
#7009 = CARTESIAN_POINT ( 'NONE',  ( -2.935661446562617183, 9.035036904803758873, 5.806742014460233747 ) ) ;
#7010 = FACE_OUTER_BOUND ( 'NONE', #18085, .T. ) ;
#7011 = CARTESIAN_POINT ( 'NONE',  ( 71.96568270381689558, 7.420530141404717394E-15, 0.000000000000000000 ) ) ;
#7012 = CARTESIAN_POINT ( 'NONE',  ( 28.99999999999999645, 29.49999999999999645, -1.500000000000000000 ) ) ;
#7013 = DIRECTION ( 'NONE',  ( 1.000000000000000000, 1.224606353822377258E-16, 0.000000000000000000 ) ) ;
#7014 = CIRCLE ( 'NONE', #14410, 5.000000000000007994 ) ;
#7015 = DIRECTION ( 'NONE',  ( 1.000000000000000000, 2.600433232233976523E-16, -0.000000000000000000 ) ) ;
#7016 = FACE_OUTER_BOUND ( 'NONE', #9821, .T. ) ;
#7017 = CARTESIAN_POINT ( 'NONE',  ( -1.999999999999996669, 45.00000000000000000, -3.000000000000000000 ) ) ;
#7018 = ORIENTED_EDGE ( 'NONE', *, *, #3056, .T. ) ;
#7019 = FACE_OUTER_BOUND ( 'NONE', #23269, .T. ) ;
#7020 = VERTEX_POINT ( 'NONE', #9308 ) ;
#7021 = EDGE_CURVE ( 'NONE', #8782, #9633, #11787, .T. ) ;
#7022 = DIRECTION ( 'NONE',  ( 0.000000000000000000, 0.000000000000000000, 1.000000000000000000 ) ) ;
#7023 = FACE_OUTER_BOUND ( 'NONE', #23036, .T. ) ;
#7024 = ORIENTED_EDGE ( 'NONE', *, *, #9722, .F. ) ;
#7025 = EDGE_LOOP ( 'NONE', ( #5943, #4747, #2188, #2363, #15621, #11771 ) ) ;
#7026 = EDGE_CURVE ( 'NONE', #22152, #20548, #4088, .T. ) ;
#7027 = FACE_OUTER_BOUND ( 'NONE', #21891, .T. ) ;
#7028 = CARTESIAN_POINT ( 'NONE',  ( -2.935661446561384391, -9.035036904804158553, -5.459589141758144137 ) ) ;
#7029 = CARTESIAN_POINT ( 'NONE',  ( -42.00000000000000000, 25.22443390181683043, -3.000000000000000000 ) ) ;
#7030 = DIRECTION ( 'NONE',  ( -0.000000000000000000, -0.000000000000000000, -1.000000000000000000 ) ) ;
#7031 = DIRECTION ( 'NONE',  ( -1.000000000000000000, -0.000000000000000000, -0.000000000000000000 ) ) ;
#7032 = DIRECTION ( 'NONE',  ( 0.000000000000000000, 0.000000000000000000, -1.000000000000000000 ) ) ;
#7033 = EDGE_LOOP ( 'NONE', ( #14398, #10796 ) ) ;
#7034 = DIRECTION ( 'NONE',  ( -0.000000000000000000, -0.000000000000000000, -1.000000000000000000 ) ) ;
#7035 = CARTESIAN_POINT ( 'NONE',  ( 20.85000000000000853, 15.03999999999999915, -27.00000000000000000 ) ) ;
#7036 = ORIENTED_EDGE ( 'NONE', *, *, #7305, .T. ) ;
#7037 = CARTESIAN_POINT ( 'NONE',  ( 27.99999999999998934, -51.00000000000000711, 0.5000000000000000000 ) ) ;
#7038 = DIRECTION ( 'NONE',  ( 0.000000000000000000, 0.000000000000000000, 1.000000000000000000 ) ) ;
#7039 =( NAMED_UNIT ( * ) PLANE_ANGLE_UNIT ( ) SI_UNIT ( $, .RADIAN. ) );
#7040 = CARTESIAN_POINT ( 'NONE',  ( 33.99999999999998579, 3.999999999999985345, 9.500000000000000000 ) ) ;
#7041 = ORIENTED_EDGE ( 'NONE', *, *, #13110, .F. ) ;
#7042 = CARTESIAN_POINT ( 'NONE',  ( -34.00000000000000000, 5.999999999999999112, 11.00000000000000000 ) ) ;
#7043 = SHAPE_REPRESENTATION ( 'Pin 2X4', ( #8005 ), #19339 ) ;
#7044 = LINE ( 'NONE', #3399, #22620 ) ;
#7045 = EDGE_LOOP ( 'NONE', ( #4933, #7112, #17015, #12718 ) ) ;
#7046 = ORIENTED_EDGE ( 'NONE', *, *, #17575, .T. ) ;
#7047 = AXIS2_PLACEMENT_3D ( 'NONE', #17780, #6795, #2762 ) ;
#7048 = CARTESIAN_POINT ( 'NONE',  ( 2.935661446561383503, 9.035036904804158553, 9.606742014460232681 ) ) ;
#7049 = CARTESIAN_POINT ( 'NONE',  ( -2.935661446562617183, 9.035036904803758873, 5.806742014460233747 ) ) ;
#7050 = VERTEX_POINT ( 'NONE', #11362 ) ;
#7051 = ORIENTED_EDGE ( 'NONE', *, *, #2179, .T. ) ;
#7052 = LINE ( 'NONE', #14483, #20704 ) ;
#7053 = ADVANCED_FACE ( 'NONE', ( #5904 ), #7718, .F. ) ;
#7054 = DIRECTION ( 'NONE',  ( -0.000000000000000000, -0.000000000000000000, -1.000000000000000000 ) ) ;
#7055 = DIRECTION ( 'NONE',  ( 0.000000000000000000, -1.000000000000000000, 0.000000000000000000 ) ) ;
#7056 = EDGE_CURVE ( 'NONE', #7965, #4778, #11248, .T. ) ;
#7057 = CYLINDRICAL_SURFACE ( 'NONE', #16838, 8.000000000000000000 ) ;
#7058 = ORIENTED_EDGE ( 'NONE', *, *, #22003, .T. ) ;
#7059 = CONICAL_SURFACE ( 'NONE', #11315, 5.024999999999998579, 0.7853981633974438381 ) ;
#7060 = AXIS2_PLACEMENT_3D ( 'NONE', #3521, #19885, #21831 ) ;
#7061 = LINE ( 'NONE', #23791, #7576 ) ;
#7062 = ORIENTED_EDGE ( 'NONE', *, *, #23282, .T. ) ;
#7063 = FILL_AREA_STYLE_COLOUR ( '', #3166 ) ;
#7064 = LINE ( 'NONE', #18069, #19234 ) ;
#7065 = AXIS2_PLACEMENT_3D ( 'NONE', #2755, #12264, #6666 ) ;
#7066 = CARTESIAN_POINT ( 'NONE',  ( -9.197647033420587093, 2.458369856709957002, -3.500931213193340330 ) ) ;
#7067 = CARTESIAN_POINT ( 'NONE',  ( 19.85000000000000142, -16.67999999999999616, 14.50000000000000000 ) ) ;
#7068 = CARTESIAN_POINT ( 'NONE',  ( 80.69295543108962931, 7.420530141404717394E-15, 0.000000000000000000 ) ) ;
#7069 = DIRECTION ( 'NONE',  ( 1.000000000000000000, 0.000000000000000000, 0.000000000000000000 ) ) ;
#7070 = VERTEX_POINT ( 'NONE', #14805 ) ;
#7071 = EDGE_CURVE ( 'NONE', #11063, #12041, #9416, .T. ) ;
#7072 = DIRECTION ( 'NONE',  ( -1.000000000000000000, -8.326672684688666165E-15, 0.000000000000000000 ) ) ;
#7073 = ORIENTED_EDGE ( 'NONE', *, *, #3005, .T. ) ;
#7074 = DIRECTION ( 'NONE',  ( -0.000000000000000000, -0.000000000000000000, -1.000000000000000000 ) ) ;
#7075 = CARTESIAN_POINT ( 'NONE',  ( 40.77574956473004164, 27.49633847812775755, 11.00000000000000000 ) ) ;
#7076 = ORIENTED_EDGE ( 'NONE', *, *, #7674, .F. ) ;
#7077 = CARTESIAN_POINT ( 'NONE',  ( -39.99999999999999289, 29.50000000000000000, -27.00000000000000000 ) ) ;
#7078 = EDGE_CURVE ( 'NONE', #6244, #23756, #9205, .T. ) ;
#7079 = DIRECTION ( 'NONE',  ( -1.000000000000000000, -1.224606353822377258E-16, -0.000000000000000000 ) ) ;
#7080 = CARTESIAN_POINT ( 'NONE',  ( 8.000000000000000000, 0.000000000000000000, -12.50000000000000000 ) ) ;
#7081=STYLED_ITEM('',(#24141),#19017);
#7082 = EDGE_CURVE ( 'NONE', #16520, #1470, #138, .T. ) ;
#7083 = DIRECTION ( 'NONE',  ( -0.000000000000000000, -0.000000000000000000, -1.000000000000000000 ) ) ;
#7084 = ADVANCED_FACE ( 'NONE', ( #1995 ), #19634, .T. ) ;
#7085 = EDGE_CURVE ( 'NONE', #2102, #3810, #16860, .T. ) ;
#7086 = AXIS2_PLACEMENT_3D ( 'NONE', #20666, #414, #18837 ) ;
#7087 = CARTESIAN_POINT ( 'NONE',  ( -14.99999999999999645, 15.50000000000000178, 7.700000000000001954 ) ) ;
#7088 = DIRECTION ( 'NONE',  ( 0.000000000000000000, 0.000000000000000000, 1.000000000000000000 ) ) ;
#7089 = CARTESIAN_POINT ( 'NONE',  ( -5.871322893123450015, -8.081182679344781405, -11.35958914175814272 ) ) ;
#7090 = ORIENTED_EDGE ( 'NONE', *, *, #10076, .F. ) ;
#7091 = EDGE_LOOP ( 'NONE', ( #9721, #7557, #20030, #10639 ) ) ;
#7092 = CYLINDRICAL_SURFACE ( 'NONE', #573, 5.000000000000000888 ) ;
#7093 = CARTESIAN_POINT ( 'NONE',  ( 40.00000000000000000, -29.50000000000000000, 27.00000000000000000 ) ) ;
#7094 = VECTOR ( 'NONE', #8618, 1000.000000000000000 ) ;
#7095 = VECTOR ( 'NONE', #18518, 1000.000000000000000 ) ;
#7096 = VECTOR ( 'NONE', #6243, 1000.000000000000000 ) ;
#7097 = ORIENTED_EDGE ( 'NONE', *, *, #23717, .F. ) ;
#7098 = PRODUCT_DEFINITION_SHAPE ( 'NONE', 'NONE',  #24109 ) ;
#7099 = CARTESIAN_POINT ( 'NONE',  ( 11.50000000000000000, 2.119223430970168298, 17.74893002550480858 ) ) ;
#7100 = AXIS2_PLACEMENT_3D ( 'NONE', #21101, #4408, #11817 ) ;
#7101 = VECTOR ( 'NONE', #13586, 1000.000000000000000 ) ;
#7102 = EDGE_CURVE ( 'NONE', #16743, #24058, #20798, .T. ) ;
#7103 = DIRECTION ( 'NONE',  ( -1.000000000000000000, 0.000000000000000000, 0.000000000000000000 ) ) ;
#7104 = ORIENTED_EDGE ( 'NONE', *, *, #16836, .T. ) ;
#7105 = CIRCLE ( 'NONE', #14495, 4.499999999999997335 ) ;
#7106 = FACE_OUTER_BOUND ( 'NONE', #6440, .T. ) ;
#7107 = CARTESIAN_POINT ( 'NONE',  ( -41.73082370883257397, -27.62204025492845361, -1.500000000000000000 ) ) ;
#7108 = DIRECTION ( 'NONE',  ( 0.000000000000000000, 0.000000000000000000, 1.000000000000000000 ) ) ;
#7109 = FACE_OUTER_BOUND ( 'NONE', #12490, .T. ) ;
#7110 = EDGE_CURVE ( 'NONE', #208, #6244, #21957, .T. ) ;
#7111 = VERTEX_POINT ( 'NONE', #20565 ) ;
#7112 = ORIENTED_EDGE ( 'NONE', *, *, #19459, .T. ) ;
#7113 = AXIS2_PLACEMENT_3D ( 'NONE', #19505, #13897, #2781 ) ;
#7114 = ORIENTED_EDGE ( 'NONE', *, *, #4520, .T. ) ;
#7115 = AXIS2_PLACEMENT_3D ( 'NONE', #11573, #19043, #2198 ) ;
#7117 = VECTOR ( 'NONE', #21111, 1000.000000000000000 ) ;
#7116 = CYLINDRICAL_SURFACE ( 'NONE', #11928, 5.000000000000000888 ) ;
#7118 = AXIS2_PLACEMENT_3D ( 'NONE', #13028, #12791, #1583 ) ;
#7119 = VECTOR ( 'NONE', #756, 1000.000000000000000 ) ;
#7120 = DIRECTION ( 'NONE',  ( 0.000000000000000000, -1.000000000000000000, 0.000000000000000000 ) ) ;
#7121 = ORIENTED_EDGE ( 'NONE', *, *, #19695, .T. ) ;
#7122 = AXIS2_PLACEMENT_3D ( 'NONE', #1131, #15993, #10497 ) ;
#7123 = DIRECTION ( 'NONE',  ( -1.000000000000000000, -1.224606353822377258E-16, -0.000000000000000000 ) ) ;
#7124 = CONICAL_SURFACE ( 'NONE', #9434, 4.172000000000008590, 0.9599310885968742602 ) ;
#7125 = ORIENTED_EDGE ( 'NONE', *, *, #3973, .T. ) ;
#7126 = DIRECTION ( 'NONE',  ( 0.5735764363510427177, -0.8191520442889941300, 1.003171929053527705E-16 ) ) ;
#7127 = LINE ( 'NONE', #3472, #20765 ) ;
#7128 = FACE_OUTER_BOUND ( 'NONE', #2299, .T. ) ;
#7129 = CARTESIAN_POINT ( 'NONE',  ( -1.499999999999999556, 0.000000000000000000, 6.000000000000000000 ) ) ;
#7130 = LINE ( 'NONE', #21901, #23080 ) ;
#7131 = AXIS2_PLACEMENT_3D ( 'NONE', #4229, #6288, #18997 ) ;
#7132 = LINE ( 'NONE', #14570, #22361 ) ;
#7133 = EDGE_CURVE ( 'NONE', #11854, #19436, #9856, .T. ) ;
#7134 = DIRECTION ( 'NONE',  ( -1.000000000000000000, 0.000000000000000000, 0.000000000000000000 ) ) ;
#7135 = VECTOR ( 'NONE', #19396, 1000.000000000000000 ) ;
#7136 = DIRECTION ( 'NONE',  ( 0.5735764363510427177, -0.8191520442889941300, 1.003171929053527705E-16 ) ) ;
#7137 = AXIS2_PLACEMENT_3D ( 'NONE', #23624, #1285, #4963 ) ;
#7138 = CIRCLE ( 'NONE', #9835, 6.050000000006051870 ) ;
#7139 = ORIENTED_EDGE ( 'NONE', *, *, #20776, .F. ) ;
#7140 = CARTESIAN_POINT ( 'NONE',  ( 8.680847955710813579, 2.820578480814259326, 8.733165578109185034 ) ) ;
#7141 = ORIENTED_EDGE ( 'NONE', *, *, #1950, .T. ) ;
#7142 = AXIS2_PLACEMENT_3D ( 'NONE', #21650, #18335, #18225 ) ;
#7143 = ADVANCED_FACE ( 'NONE', ( #5433 ), #7600, .F. ) ;
#7144 = AXIS2_PLACEMENT_3D ( 'NONE', #2937, #12314, #23560 ) ;
#7145 = DIRECTION ( 'NONE',  ( -0.000000000000000000, -0.000000000000000000, 1.000000000000000000 ) ) ;
#7146 = ORIENTED_EDGE ( 'NONE', *, *, #3862, .F. ) ;
#7147 = ORIENTED_EDGE ( 'NONE', *, *, #5020, .T. ) ;
#7148 = CARTESIAN_POINT ( 'NONE',  ( -9.096421271198437353, 2.534255564213257372, -12.07085958584578300 ) ) ;
#7149 = CARTESIAN_POINT ( 'NONE',  ( -9.500000000000211386, 3.086737114211961064, -4.959589141758145026 ) ) ;
#7150 = DIRECTION ( 'NONE',  ( 0.000000000000000000, 0.000000000000000000, 1.000000000000000000 ) ) ;
#7151 = CARTESIAN_POINT ( 'NONE',  ( -31.74999999999995737, 0.000000000000000000, 5.000000000000000888 ) ) ;
#7152 = FACE_OUTER_BOUND ( 'NONE', #20387, .T. ) ;
#7153 = VECTOR ( 'NONE', #10516, 1000.000000000000000 ) ;
#7154 = DIRECTION ( 'NONE',  ( 0.000000000000000000, 0.000000000000000000, 1.000000000000000000 ) ) ;
#7155 = VECTOR ( 'NONE', #8467, 1000.000000000000000 ) ;
#7156 = CARTESIAN_POINT ( 'NONE',  ( 7.685661446562381371, -5.583959896777971110, -7.006742014460233037 ) ) ;
#7157 = AXIS2_PLACEMENT_3D ( 'NONE', #5803, #17134, #18623 ) ;
#7158 = VECTOR ( 'NONE', #23848, 1000.000000000000000 ) ;
#7159 = EDGE_CURVE ( 'NONE', #8434, #145, #11011, .T. ) ;
#7160 = ORIENTED_EDGE ( 'NONE', *, *, #684, .T. ) ;
#7161 = DIRECTION ( 'NONE',  ( 0.000000000000000000, 0.000000000000000000, -1.000000000000000000 ) ) ;
#7162 = CARTESIAN_POINT ( 'NONE',  ( -18.49999999999999645, -15.23000000000000220, -27.00000000000000000 ) ) ;
#7163 = AXIS2_PLACEMENT_3D ( 'NONE', #16543, #7488, #16767 ) ;
#7164 = CARTESIAN_POINT ( 'NONE',  ( 0.000000000000000000, 0.000000000000000000, 0.000000000000000000 ) ) ;
#7165 = DIRECTION ( 'NONE',  ( -1.000000000000000000, -1.224606353822377258E-16, -0.000000000000000000 ) ) ;
#7166 = AXIS2_PLACEMENT_3D ( 'NONE', #8623, #6461, #4883 ) ;
#7167 = CARTESIAN_POINT ( 'NONE',  ( -1.029124893018731811E-15, 45.00000000000000000, -22.79827876194487857 ) ) ;
#7168 = ADVANCED_FACE ( 'NONE', ( #9556 ), #18485, .F. ) ;
#7169 = ORIENTED_EDGE ( 'NONE', *, *, #5335, .T. ) ;
#7170 = LINE ( 'NONE', #22074, #12581 ) ;
#7171 = DIRECTION ( 'NONE',  ( -0.000000000000000000, -0.000000000000000000, -1.000000000000000000 ) ) ;
#7172 = ORIENTED_EDGE ( 'NONE', *, *, #17690, .F. ) ;
#7173 = ORIENTED_EDGE ( 'NONE', *, *, #21696, .T. ) ;
#7174 = CARTESIAN_POINT ( 'NONE',  ( -7.685661446561619314, -5.583959896779019161, 8.406742014460233392 ) ) ;
#7175 = CARTESIAN_POINT ( 'NONE',  ( 9.500000000000209610, -3.086737114211962396, 7.106742014460232681 ) ) ;
#7176 = VERTEX_POINT ( 'NONE', #3723 ) ;
#7177 = ORIENTED_EDGE ( 'NONE', *, *, #5135, .T. ) ;
#7178 =( NAMED_UNIT ( * ) SI_UNIT ( $, .STERADIAN. ) SOLID_ANGLE_UNIT ( ) );
#7179 = AXIS2_PLACEMENT_3D ( 'NONE', #13413, #10221, #737 ) ;
#7180 = FACE_OUTER_BOUND ( 'NONE', #1652, .T. ) ;
#7181 = CARTESIAN_POINT ( 'NONE',  ( -40.00000000000000000, -28.80990663662251450, 11.00000000000000000 ) ) ;
#7182 = AXIS2_PLACEMENT_3D ( 'NONE', #22029, #20078, #12485 ) ;
#7183 = AXIS2_PLACEMENT_3D ( 'NONE', #3713, #11124, #22505 ) ;
#7184 = VECTOR ( 'NONE', #20689, 1000.000000000000000 ) ;
#7185 = DIRECTION ( 'NONE',  ( -1.000000000000000000, -1.224606353822377258E-16, -0.000000000000000000 ) ) ;
#7186 = DIRECTION ( 'NONE',  ( 0.000000000000000000, 0.000000000000000000, -1.000000000000000000 ) ) ;
#7187 = CARTESIAN_POINT ( 'NONE',  ( 2.935661446561383503, 9.035036904804158553, -10.45958914175814414 ) ) ;
#7188 = ORIENTED_EDGE ( 'NONE', *, *, #8170, .F. ) ;
#7189 = DIRECTION ( 'NONE',  ( -0.000000000000000000, -0.000000000000000000, -1.000000000000000000 ) ) ;
#7190 = DIRECTION ( 'NONE',  ( 0.000000000000000000, 1.000000000000000000, 0.000000000000000000 ) ) ;
#7191 = DIRECTION ( 'NONE',  ( -1.000000000000000000, 0.000000000000000000, 0.000000000000000000 ) ) ;
#7192 = DIRECTION ( 'NONE',  ( 0.000000000000000000, 0.000000000000000000, -1.000000000000000000 ) ) ;
#7193 =( BOUNDED_CURVE ( )  B_SPLINE_CURVE ( 2, ( #11885, #15538, #23005, #17500, #6652, #2632, #2508, #10045, #4337, #1055, #801 ),
 .UNSPECIFIED., .F., .F. ) 
 B_SPLINE_CURVE_WITH_KNOTS ( ( 3, 2, 2, 2, 2, 3 ),
 ( 0.4999999999999999445, 0.5200000000000000178, 0.5400000000000000355, 0.5600000000000000533, 0.5800000000000000711, 0.6000000000000000888 ),
 .UNSPECIFIED. ) 
 CURVE ( )  GEOMETRIC_REPRESENTATION_ITEM ( )  RATIONAL_B_SPLINE_CURVE ( ( 1.000000000000000000, 0.9510565162951533091, 1.000000000000000000, 0.9510565162951535312, 1.000000000000000000, 0.9510565162951535312, 1.000000000000000000, 0.9510565162951535312, 1.000000000000000000, 0.9510565162951533091, 1.000000000000000222 ) ) 
 REPRESENTATION_ITEM ( '' )  );
#7194 = CIRCLE ( 'NONE', #19289, 1.000000000000000888 ) ;
#7195 = FACE_OUTER_BOUND ( 'NONE', #19456, .T. ) ;
#7196 = EDGE_CURVE ( 'NONE', #13441, #2834, #4045, .T. ) ;
#7197 = EDGE_CURVE ( 'NONE', #5210, #2386, #13217, .T. ) ;
#7198 = CIRCLE ( 'NONE', #14214, 6.050000000006050094 ) ;
#7199 = CARTESIAN_POINT ( 'NONE',  ( -14.98950073861089294, 0.6491375924673337128, 9.483449329262338523 ) ) ;
#7200 = EDGE_LOOP ( 'NONE', ( #9715, #8346, #15531, #14957, #16512 ) ) ;
#7201 = DIRECTION ( 'NONE',  ( -0.000000000000000000, -0.000000000000000000, 1.000000000000000000 ) ) ;
#7202 = EDGE_LOOP ( 'NONE', ( #2302, #12834, #13885, #19772 ) ) ;
#7203 = LINE ( 'NONE', #12690, #1684 ) ;
#7204 = EDGE_LOOP ( 'NONE', ( #8521, #5588, #18365, #9618 ) ) ;
#7205 = FACE_BOUND ( 'NONE', #18325, .T. ) ;
#7206 = VECTOR ( 'NONE', #21805, 1000.000000000000000 ) ;
#7207 = CARTESIAN_POINT ( 'NONE',  ( 23.00000000000000000, 0.000000000000000000, 0.000000000000000000 ) ) ;
#7208 = DIRECTION ( 'NONE',  ( 1.000000000000000000, -0.000000000000000000, -0.000000000000000000 ) ) ;
#7209 = ORIENTED_EDGE ( 'NONE', *, *, #22125, .F. ) ;
#7210 = CARTESIAN_POINT ( 'NONE',  ( 0.000000000000000000, 0.000000000000000000, -1.500000000000000000 ) ) ;
#7211 = CARTESIAN_POINT ( 'NONE',  ( -31.74999999999995737, 6.123233995736767268E-16, -5.000000000000000888 ) ) ;
#7212 = AXIS2_PLACEMENT_3D ( 'NONE', #21018, #405, #7811 ) ;
#7213 = EDGE_CURVE ( 'NONE', #9993, #12069, #3953, .T. ) ;
#7214 = CARTESIAN_POINT ( 'NONE',  ( -2.935661446562617183, 9.035036904803758873, -8.659589141758143427 ) ) ;
#7215 = ORIENTED_EDGE ( 'NONE', *, *, #22597, .F. ) ;
#7216 = AXIS2_PLACEMENT_3D ( 'NONE', #17554, #1110, #12180 ) ;
#7217 = ORIENTED_EDGE ( 'NONE', *, *, #12294, .F. ) ;
#7218 = CARTESIAN_POINT ( 'NONE',  ( -6.153822176767817416E-13, 9.500000000000000000, -3.568914004820086916 ) ) ;
#7219 = CARTESIAN_POINT ( 'NONE',  ( -41.73082370883257397, -27.62204025492845361, -3.000000000000000000 ) ) ;
#7220 = AXIS2_PLACEMENT_3D ( 'NONE', #9979, #21233, #14028 ) ;
#7221 = CYLINDRICAL_SURFACE ( 'NONE', #17853, 9.999999999999998224 ) ;
#7222 = CARTESIAN_POINT ( 'NONE',  ( 31.10231664966676846, -45.36128193761570770, 27.00000000000000000 ) ) ;
#7223 = ADVANCED_FACE ( 'NONE', ( #17241 ), #15412, .F. ) ;
#7224 = AXIS2_PLACEMENT_3D ( 'NONE', #16944, #18667, #13403 ) ;
#7225 = AXIS2_PLACEMENT_3D ( 'NONE', #17421, #10079, #719 ) ;
#7226 = ADVANCED_FACE ( 'NONE', ( #17742 ), #18076, .F. ) ;
#7227 = ORIENTED_EDGE ( 'NONE', *, *, #19024, .T. ) ;
#7228 = ADVANCED_FACE ( 'NONE', ( #2732 ), #15644, .F. ) ;
#7229 = DIRECTION ( 'NONE',  ( -5.501724186093582121E-16, 1.000000000000000000, 0.000000000000000000 ) ) ;
#7230 = CARTESIAN_POINT ( 'NONE',  ( -18.50000000000000000, 15.23000000000000220, 27.00000000000000000 ) ) ;
#7231 = VERTEX_POINT ( 'NONE', #21410 ) ;
#7232 = CARTESIAN_POINT ( 'NONE',  ( -7.685661446562381371, 5.583959896777970222, -10.00674201446023481 ) ) ;
#7233 = CARTESIAN_POINT ( 'NONE',  ( -29.00000000000000000, -29.49999999999999645, 0.000000000000000000 ) ) ;
#7234 = DIRECTION ( 'NONE',  ( -1.000000000000000000, -1.224606353822377258E-16, -0.000000000000000000 ) ) ;
#7235 = CARTESIAN_POINT ( 'NONE',  ( 0.000000000000000000, 0.000000000000000000, 27.00000000000000000 ) ) ;
#7236 = VECTOR ( 'NONE', #20008, 1000.000000000000000 ) ;
#7237 = CARTESIAN_POINT ( 'NONE',  ( 5.365059087799946447, -7.384370330706356178, 6.333165578109187344 ) ) ;
#7238 = ORIENTED_EDGE ( 'NONE', *, *, #10561, .F. ) ;
#7239 = EDGE_LOOP ( 'NONE', ( #14860, #19511, #23094, #23331 ) ) ;
#7240 = CIRCLE ( 'NONE', #13475, 6.050000000006050094 ) ;
#7241 = VERTEX_POINT ( 'NONE', #4324 ) ;
#7242 = AXIS2_PLACEMENT_3D ( 'NONE', #6154, #21037, #11363 ) ;
#7243 = VERTEX_POINT ( 'NONE', #13593 ) ;
#7244 = VERTEX_POINT ( 'NONE', #10287 ) ;
#7245 = CARTESIAN_POINT ( 'NONE',  ( 41.50000000000000000, 28.80990663662250739, 11.00000000000000000 ) ) ;
#7246 = EDGE_CURVE ( 'NONE', #10822, #3540, #9467, .T. ) ;
#7247 = CARTESIAN_POINT ( 'NONE',  ( -9.500000000000202505, 3.086737114211975275, 10.10674201446023268 ) ) ;
#7248 = ORIENTED_EDGE ( 'NONE', *, *, #6080, .F. ) ;
#7249 = LINE ( 'NONE', #6777, #3290 ) ;
#7250 = ORIENTED_EDGE ( 'NONE', *, *, #23660, .T. ) ;
#7251 = AXIS2_PLACEMENT_3D ( 'NONE', #6193, #12394, #16294 ) ;
#7252 = AXIS2_PLACEMENT_3D ( 'NONE', #714, #19384, #2657 ) ;
#7253 = EDGE_CURVE ( 'NONE', #17283, #23345, #2473, .T. ) ;
#7254 = FACE_OUTER_BOUND ( 'NONE', #10883, .T. ) ;
#7255 = EDGE_CURVE ( 'NONE', #17900, #10822, #5211, .T. ) ;
#7256 = FACE_OUTER_BOUND ( 'NONE', #10322, .T. ) ;
#7257 = CYLINDRICAL_SURFACE ( 'NONE', #2085, 1.999999999999994449 ) ;
#7258 = AXIS2_PLACEMENT_3D ( 'NONE', #1481, #1112, #10587 ) ;
#7259 = ORIENTED_EDGE ( 'NONE', *, *, #13323, .T. ) ;
#7260 = DIRECTION ( 'NONE',  ( 0.000000000000000000, -0.2817325568414367765, 0.9594929736144953702 ) ) ;
#7261 = CARTESIAN_POINT ( 'NONE',  ( -42.00000000000000711, 26.82133436441678498, 12.00000000000000000 ) ) ;
#7262 = CARTESIAN_POINT ( 'NONE',  ( -40.66734255040738333, 26.56420859267091927, -1.500000000000000000 ) ) ;
#7263 = ORIENTED_EDGE ( 'NONE', *, *, #18054, .F. ) ;
#7264 = ORIENTED_EDGE ( 'NONE', *, *, #17125, .T. ) ;
#7265 = CARTESIAN_POINT ( 'NONE',  ( -5.365059087798939252, -7.384370330707086261, 7.933165578109187877 ) ) ;
#7266 = EDGE_LOOP ( 'NONE', ( #890, #6587, #22467, #11541 ) ) ;
#7267 = CIRCLE ( 'NONE', #5729, 5.000000000000007994 ) ;
#7268 = APPLICATION_PROTOCOL_DEFINITION ( 'draft international standard', 'automotive_design', 1998, #11474 ) ;
#7269 = FACE_OUTER_BOUND ( 'NONE', #8599, .T. ) ;
#7270 = AXIS2_PLACEMENT_3D ( 'NONE', #21271, #6378, #19439 ) ;
#7271 = ORIENTED_EDGE ( 'NONE', *, *, #2239, .F. ) ;
#7272 = ORIENTED_EDGE ( 'NONE', *, *, #2639, .T. ) ;
#7273 = CARTESIAN_POINT ( 'NONE',  ( -34.02499999999999858, -29.50000000000000000, -3.000000000000000000 ) ) ;
#7274 = CARTESIAN_POINT ( 'NONE',  ( -7.022953521754877748, -5.102474405760673015, -9.833165578109188232 ) ) ;
#7275 = CIRCLE ( 'NONE', #19715, 4.249999999999996447 ) ;
#7276 = DIRECTION ( 'NONE',  ( 0.000000000000000000, -1.000000000000000000, 0.000000000000000000 ) ) ;
#7277 = CARTESIAN_POINT ( 'NONE',  ( -34.10000000000000142, -29.50000000000001066, 27.00000000000000000 ) ) ;
#7278 = CARTESIAN_POINT ( 'NONE',  ( 23.84999999999999432, -15.03999999999999559, -25.00000000000000000 ) ) ;
#7279 = CARTESIAN_POINT ( 'NONE',  ( 69.05659179472598908, 7.420530141404717394E-15, 0.000000000000000000 ) ) ;
#7280 = ORIENTED_EDGE ( 'NONE', *, *, #20717, .F. ) ;
#7281 = CARTESIAN_POINT ( 'NONE',  ( -31.74999999999995737, 0.000000000000000000, 0.000000000000000000 ) ) ;
#7282 = DIRECTION ( 'NONE',  ( 0.000000000000000000, -1.224646799147353207E-16, 1.000000000000000000 ) ) ;
#7283 = ADVANCED_FACE ( 'NONE', ( #7964 ), #19344, .F. ) ;
#7284 = DIRECTION ( 'NONE',  ( 0.000000000000000000, 0.000000000000000000, -1.000000000000000000 ) ) ;
#7285 = CARTESIAN_POINT ( 'NONE',  ( -42.00000000000000711, 26.82133436441678498, 11.00000000000000000 ) ) ;
#7286 = DIRECTION ( 'NONE',  ( -0.000000000000000000, -0.000000000000000000, -1.000000000000000000 ) ) ;
#7287 = AXIS2_PLACEMENT_3D ( 'NONE', #18895, #11288, #5727 ) ;
#7288 = LINE ( 'NONE', #14728, #10691 ) ;
#7289 = CARTESIAN_POINT ( 'NONE',  ( -36.00000000000000711, -51.00000000000000711, 0.5000000000000000000 ) ) ;
#7290 = CARTESIAN_POINT ( 'NONE',  ( 78.36363636363637397, 7.491529369508391930E-15, 0.000000000000000000 ) ) ;
#7291 = EDGE_LOOP ( 'NONE', ( #1420, #17515, #18907, #180 ) ) ;
#7292 = ORIENTED_EDGE ( 'NONE', *, *, #1604, .F. ) ;
#7293 = CARTESIAN_POINT ( 'NONE',  ( 2.935661446561383503, 9.035036904804158553, 7.606742014460233570 ) ) ;
#7294 = EDGE_LOOP ( 'NONE', ( #18141, #6851, #9569, #3555, #2313 ) ) ;
#7295 = EDGE_LOOP ( 'NONE', ( #21390, #19438, #22307, #9700 ) ) ;
#7296 =( NAMED_UNIT ( * ) SI_UNIT ( $, .STERADIAN. ) SOLID_ANGLE_UNIT ( ) );
#7297 = CYLINDRICAL_SURFACE ( 'NONE', #12669, 11.68650000001168721 ) ;
#7298 = DIRECTION ( 'NONE',  ( -1.000000000000000000, 0.000000000000000000, 0.000000000000000000 ) ) ;
#7299 = DIRECTION ( 'NONE',  ( 1.000000000000000000, 1.224606353822377258E-16, 0.000000000000000000 ) ) ;
#7300 = EDGE_CURVE ( 'NONE', #6647, #21329, #8315, .T. ) ;
#7301 = CARTESIAN_POINT ( 'NONE',  ( 34.10000000000000142, 29.50000000000000355, 11.50000000000000000 ) ) ;
#7302 = CARTESIAN_POINT ( 'NONE',  ( 10.00000000000000000, 8.000000000000000000, 0.000000000000000000 ) ) ;
#7303 = CARTESIAN_POINT ( 'NONE',  ( 27.89784171216407316, -41.49349862090490149, -3.000000000000000000 ) ) ;
#7304 = EDGE_CURVE ( 'NONE', #17812, #20236, #20927, .T. ) ;
#7305 = EDGE_CURVE ( 'NONE', #14307, #7839, #11808, .T. ) ;
#7306 = ORIENTED_EDGE ( 'NONE', *, *, #21456, .F. ) ;
#7307 = EDGE_CURVE ( 'NONE', #15333, #10731, #2361, .T. ) ;
#7308 = LINE ( 'NONE', #23041, #9532 ) ;
#7309 =( NAMED_UNIT ( * ) PLANE_ANGLE_UNIT ( ) SI_UNIT ( $, .RADIAN. ) );
#7310 = DIRECTION ( 'NONE',  ( -0.000000000000000000, -0.000000000000000000, -1.000000000000000000 ) ) ;
#7311 = DIRECTION ( 'NONE',  ( -1.000000000000000000, 0.000000000000000000, 0.000000000000000000 ) ) ;
#7312 = CARTESIAN_POINT ( 'NONE',  ( -5.622572944242077574E-13, 8.680847955711007202, -3.133165578109187610 ) ) ;
#7313 = DIRECTION ( 'NONE',  ( -1.000000000000000000, 0.000000000000000000, -0.000000000000000000 ) ) ;
#7314 = CARTESIAN_POINT ( 'NONE',  ( 8.680847955710813579, 2.820578480814259326, -10.73316557810918503 ) ) ;
#7315 = VECTOR ( 'NONE', #21699, 999.9999999999998863 ) ;
#7316 = CARTESIAN_POINT ( 'NONE',  ( -35.99999999999995026, 59.99999999999998579, 0.000000000000000000 ) ) ;
#7317 = AXIS2_PLACEMENT_3D ( 'NONE', #6878, #21762, #19819 ) ;
#7318 = ORIENTED_EDGE ( 'NONE', *, *, #19156, .F. ) ;
#7319 = CARTESIAN_POINT ( 'NONE',  ( 79.23840997654417606, 5.000000000000007105, 6.123233995736765296E-16 ) ) ;
#7320 = ORIENTED_EDGE ( 'NONE', *, *, #3154, .F. ) ;
#7321 = LINE ( 'NONE', #3663, #1309 ) ;
#7322 = VERTEX_POINT ( 'NONE', #6152 ) ;
#7323 = FACE_OUTER_BOUND ( 'NONE', #20702, .T. ) ;
#7324 = CARTESIAN_POINT ( 'NONE',  ( 3.000000000000000888, 8.485281374238567764, 80.99999999999998579 ) ) ;
#7325 = DIRECTION ( 'NONE',  ( -0.000000000000000000, 0.000000000000000000, -1.000000000000000000 ) ) ;
#7326 = EDGE_CURVE ( 'NONE', #12531, #22492, #10148, .T. ) ;
#7327 = ADVANCED_FACE ( 'NONE', ( #23252 ), #15785, .F. ) ;
#7328 = TOROIDAL_SURFACE ( 'NONE', #18247, 10.00000000000000888, 1.000000000000000000 ) ;
#7329 = AXIS2_PLACEMENT_3D ( 'NONE', #22002, #1738, #12580 ) ;
#7330 = CARTESIAN_POINT ( 'NONE',  ( -2.935661446562617183, 9.035036904803758873, -4.659589141758143427 ) ) ;
#7331 = ORIENTED_EDGE ( 'NONE', *, *, #20280, .F. ) ;
#7332 = VERTEX_POINT ( 'NONE', #4456 ) ;
#7333 = DIRECTION ( 'NONE',  ( -0.000000000000000000, -0.000000000000000000, -1.000000000000000000 ) ) ;
#7334 = ORIENTED_EDGE ( 'NONE', *, *, #20014, .F. ) ;
#7335 = FACE_OUTER_BOUND ( 'NONE', #14225, .T. ) ;
#7336 = ORIENTED_EDGE ( 'NONE', *, *, #7892, .T. ) ;
#7337 = CIRCLE ( 'NONE', #20633, 5.100000000000000533 ) ;
#7338 = CARTESIAN_POINT ( 'NONE',  ( 11.49999999999999822, 12.02595010061972403, -13.22467954916274913 ) ) ;
#7339 = CARTESIAN_POINT ( 'NONE',  ( 0.000000000000000000, 0.000000000000000000, 0.000000000000000000 ) ) ;
#7340 = ORIENTED_EDGE ( 'NONE', *, *, #17211, .T. ) ;
#7341 = DIRECTION ( 'NONE',  ( -1.000000000000000000, 0.000000000000000000, 0.000000000000000000 ) ) ;
#7342 = PLANE ( 'NONE',  #4930 ) ;
#7343 = CARTESIAN_POINT ( 'NONE',  ( 2.682529543899157876, 8.255977015246598327, 5.033165578109189298 ) ) ;
#7344 = ORIENTED_EDGE ( 'NONE', *, *, #3459, .T. ) ;
#7345 = EDGE_LOOP ( 'NONE', ( #6328, #11255 ) ) ;
#7346 = ORIENTED_EDGE ( 'NONE', *, *, #12807, .F. ) ;
#7347 = EDGE_CURVE ( 'NONE', #11891, #13330, #23147, .T. ) ;
#7348 = EDGE_LOOP ( 'NONE', ( #23467, #13145, #10441, #19141 ) ) ;
#7349 = CONTEXT_DEPENDENT_SHAPE_REPRESENTATION ( #2962, #14305 ) ;
#7350 = EDGE_CURVE ( 'NONE', #8857, #7831, #12598, .T. ) ;
#7351 = EDGE_LOOP ( 'NONE', ( #12043, #10402, #794, #137 ) ) ;
#7352 = LINE ( 'NONE', #12730, #11129 ) ;
#7353 = CLOSED_SHELL ( 'NONE', ( #603, #12731, #5063, #560, #20519, #19760, #17951, #18884, #7975, #245, #11020, #20683, #20110, #13869 ) ) ;
#7354 = EDGE_CURVE ( 'NONE', #8169, #24045, #13841, .T. ) ;
#7355 = CARTESIAN_POINT ( 'NONE',  ( 81.85249911436491743, -1.078520768856852078E-29, 5.000000000000007994 ) ) ;
#7356 = ORIENTED_EDGE ( 'NONE', *, *, #6049, .T. ) ;
#7357 = EDGE_LOOP ( 'NONE', ( #8810, #10659, #6641, #19790 ) ) ;
#7358 = DIRECTION ( 'NONE',  ( 0.4828336235133057208, -0.8757121056631633760, 0.000000000000000000 ) ) ;
#7359 = DIRECTION ( 'NONE',  ( 0.000000000000000000, 0.000000000000000000, -1.000000000000000000 ) ) ;
#7360 = ORIENTED_EDGE ( 'NONE', *, *, #15103, .T. ) ;
#7361 = LINE ( 'NONE', #21900, #5519 ) ;
#7362 = CARTESIAN_POINT ( 'NONE',  ( 40.89823313241238623, -26.41789760203348081, 27.00000000000000000 ) ) ;
#7363 = FACE_OUTER_BOUND ( 'NONE', #19145, .T. ) ;
#7364 = DIRECTION ( 'NONE',  ( -1.000000000000000000, 2.600433232233976523E-16, 0.000000000000000000 ) ) ;
#7365 = DIRECTION ( 'NONE',  ( -0.000000000000000000, -0.000000000000000000, -1.000000000000000000 ) ) ;
#7366 = CARTESIAN_POINT ( 'NONE',  ( -28.27483331787888687, 41.23752903419610050, 0.000000000000000000 ) ) ;
#7367 = ORIENTED_EDGE ( 'NONE', *, *, #23692, .F. ) ;
#7368 = ORIENTED_EDGE ( 'NONE', *, *, #15668, .F. ) ;
#7369 = CARTESIAN_POINT ( 'NONE',  ( -5.365059087799947335, 7.384370330706355290, 11.33316557810918468 ) ) ;
#7370 = ADVANCED_FACE ( 'NONE', ( #6643 ), #4384, .F. ) ;
#7371 = ORIENTED_EDGE ( 'NONE', *, *, #2298, .T. ) ;
#7372 = CIRCLE ( 'NONE', #15553, 4.499999999999997335 ) ;
#7373 = APPLICATION_PROTOCOL_DEFINITION ( 'draft international standard', 'automotive_design', 1998, #8195 ) ;
#7374 = ORIENTED_EDGE ( 'NONE', *, *, #12074, .F. ) ;
#7375 = ORIENTED_EDGE ( 'NONE', *, *, #9688, .F. ) ;
#7376 = ADVANCED_FACE ( 'NONE', ( #10637 ), #3602, .T. ) ;
#7377 = DIRECTION ( 'NONE',  ( -0.000000000000000000, -0.000000000000000000, -1.000000000000000000 ) ) ;
#7378 = CARTESIAN_POINT ( 'NONE',  ( -5.365059087798939252, -7.384370330707086261, -7.933165578109187877 ) ) ;
#7379 = EDGE_CURVE ( 'NONE', #19404, #8356, #23827, .T. ) ;
#7380 = ORIENTED_EDGE ( 'NONE', *, *, #16476, .F. ) ;
#7381 = CARTESIAN_POINT ( 'NONE',  ( 68.18181818181818699, 7.491529369508391930E-15, 0.000000000000000000 ) ) ;
#7382 = CARTESIAN_POINT ( 'NONE',  ( 23.00000000000000000, -13.61176534793449200, 4.089617900950054619 ) ) ;
#7383 = CARTESIAN_POINT ( 'NONE',  ( -31.74999999999995737, 0.000000000000000000, 0.000000000000000000 ) ) ;
#7384 = CARTESIAN_POINT ( 'NONE',  ( 42.00000000000000000, 5.999999999999986677, 11.00000000000000000 ) ) ;
#7385 = VERTEX_POINT ( 'NONE', #19826 ) ;
#7386 = CARTESIAN_POINT ( 'NONE',  ( -39.00000000000000711, -29.49999999999999645, 11.00000000000000000 ) ) ;
#7387 = ORIENTED_EDGE ( 'NONE', *, *, #9149, .F. ) ;
#7388 = VECTOR ( 'NONE', #20372, 1000.000000000000000 ) ;
#7389 = ORIENTED_EDGE ( 'NONE', *, *, #7674, .T. ) ;
#7390 = CYLINDRICAL_SURFACE ( 'NONE', #9401, 11.24716442891539714 ) ;
#7391 = CARTESIAN_POINT ( 'NONE',  ( -43.50000000000000711, 25.84341543330624091, 0.000000000000000000 ) ) ;
#7392 = DIRECTION ( 'NONE',  ( -1.000000000000000000, -0.000000000000000000, -0.000000000000000000 ) ) ;
#7393 = DIRECTION ( 'NONE',  ( 1.000000000000000000, 0.000000000000000000, -0.000000000000000000 ) ) ;
#7394 = CARTESIAN_POINT ( 'NONE',  ( 77.48886275072855767, 5.000000000000015987, 0.000000000000000000 ) ) ;
#7395 = FACE_OUTER_BOUND ( 'NONE', #1439, .T. ) ;
#7396 = ORIENTED_EDGE ( 'NONE', *, *, #4062, .F. ) ;
#7397 = ADVANCED_FACE ( 'NONE', ( #23374 ), #3098, .F. ) ;
#7398 = ORIENTED_EDGE ( 'NONE', *, *, #16266, .T. ) ;
#7399 = CARTESIAN_POINT ( 'NONE',  ( -2.935661446562617183, 9.035036904803758873, 9.806742014460233747 ) ) ;
#7400 = ORIENTED_EDGE ( 'NONE', *, *, #8322, .F. ) ;
#7401 = ORIENTED_EDGE ( 'NONE', *, *, #3296, .F. ) ;
#7402 = ORIENTED_EDGE ( 'NONE', *, *, #12510, .T. ) ;
#7403 = CARTESIAN_POINT ( 'NONE',  ( 9.500000000000209610, -3.086737114211962396, 9.959589141758144137 ) ) ;
#7404 = EDGE_CURVE ( 'NONE', #7070, #2036, #1287, .T. ) ;
#7405 = DIRECTION ( 'NONE',  ( 0.000000000000000000, 0.000000000000000000, -1.000000000000000000 ) ) ;
#7406 = LINE ( 'NONE', #115, #11486 ) ;
#7407 = FACE_OUTER_BOUND ( 'NONE', #1385, .T. ) ;
#7408 = EDGE_LOOP ( 'NONE', ( #16048, #11106 ) ) ;
#7409 = CARTESIAN_POINT ( 'NONE',  ( -29.00000000000000000, -29.49999999999999645, 11.50000000000000000 ) ) ;
#7410 = DIRECTION ( 'NONE',  ( -1.000000000000000000, 0.000000000000000000, 0.000000000000000000 ) ) ;
#7411 = CARTESIAN_POINT ( 'NONE',  ( -17.49066032632880763, 9.200828712690867661, -2.414248458042551171 ) ) ;
#7412 = CARTESIAN_POINT ( 'NONE',  ( 5.378177448618336243, 0.000000000000000000, -9.747164428915397139 ) ) ;
#7413 = VECTOR ( 'NONE', #17151, 1000.000000000000000 ) ;
#7414 = CARTESIAN_POINT ( 'NONE',  ( 14.51962751333974389, 3.765689428759031010, -8.721787840009197268 ) ) ;
#7415 = ADVANCED_FACE ( 'NONE', ( #10520 ), #18110, .F. ) ;
#7416 = FACE_OUTER_BOUND ( 'NONE', #2068, .T. ) ;
#7417 = ORIENTED_EDGE ( 'NONE', *, *, #3377, .F. ) ;
#7418 = FACE_OUTER_BOUND ( 'NONE', #22241, .T. ) ;
#7419 = VERTEX_POINT ( 'NONE', #8930 ) ;
#7420 = EDGE_CURVE ( 'NONE', #24058, #22047, #12592, .T. ) ;
#7421 = CARTESIAN_POINT ( 'NONE',  ( 29.00000000000000000, 29.50000000000000355, 11.00000000000000000 ) ) ;
#7422 = EDGE_LOOP ( 'NONE', ( #15684, #229, #6772, #7336 ) ) ;
#7423 = DIRECTION ( 'NONE',  ( 0.000000000000000000, 0.000000000000000000, 1.000000000000000000 ) ) ;
#7424 = CARTESIAN_POINT ( 'NONE',  ( -28.00000000000000355, -51.00000000000000711, 0.000000000000000000 ) ) ;
#7425 = EDGE_CURVE ( 'NONE', #11436, #11499, #5553, .T. ) ;
#7426 = CARTESIAN_POINT ( 'NONE',  ( 79.23840997654417606, 7.420530141404717394E-15, 0.000000000000000000 ) ) ;
#7427 = EDGE_CURVE ( 'NONE', #3246, #7598, #1405, .T. ) ;
#7428 = AXIS2_PLACEMENT_3D ( 'NONE', #3168, #5372, #12797 ) ;
#7429 = CARTESIAN_POINT ( 'NONE',  ( -41.00000000000000000, -6.000000000000000888, 11.00000000000000000 ) ) ;
#7430 = AXIS2_PLACEMENT_3D ( 'NONE', #10313, #10174, #21551 ) ;
#7431 = CARTESIAN_POINT ( 'NONE',  ( 5.871322893123449127, 8.081182679344781405, -8.359589141758144493 ) ) ;
#7432 = ORIENTED_EDGE ( 'NONE', *, *, #14100, .T. ) ;
#7433 = ORIENTED_EDGE ( 'NONE', *, *, #11566, .F. ) ;
#7434 = CARTESIAN_POINT ( 'NONE',  ( -14.51962751333974389, 3.765689428759031010, 27.00000000000000000 ) ) ;
#7435 = ORIENTED_EDGE ( 'NONE', *, *, #10244, .T. ) ;
#7436 = PRESENTATION_STYLE_ASSIGNMENT (( #12823 ) ) ;
#7437 = ORIENTED_EDGE ( 'NONE', *, *, #3528, .T. ) ;
#7438 = EDGE_CURVE ( 'NONE', #18281, #7627, #7105, .T. ) ;
#7439 = DIRECTION ( 'NONE',  ( 1.000000000000000000, 5.501724186093582121E-16, 0.000000000000000000 ) ) ;
#7440 = CARTESIAN_POINT ( 'NONE',  ( -31.74999999999995737, 0.000000000000000000, 0.000000000000000000 ) ) ;
#7441 = CARTESIAN_POINT ( 'NONE',  ( 77.78386452199872281, 7.420530141404717394E-15, 0.000000000000000000 ) ) ;
#7442 = ORIENTED_EDGE ( 'NONE', *, *, #21625, .F. ) ;
#7443 = LINE ( 'NONE', #15128, #12623 ) ;
#7444 = EDGE_CURVE ( 'NONE', #5402, #8867, #3991, .T. ) ;
#7445 = CYLINDRICAL_SURFACE ( 'NONE', #14894, 5.000000000000000888 ) ;
#7446 = DIRECTION ( 'NONE',  ( 0.000000000000000000, -1.000000000000000000, 0.000000000000000000 ) ) ;
#7447 = CARTESIAN_POINT ( 'NONE',  ( 0.000000000000000000, 0.000000000000000000, 12.50000000000000000 ) ) ;
#7448 = EDGE_CURVE ( 'NONE', #20529, #19325, #21881, .T. ) ;
#7449 = VERTEX_POINT ( 'NONE', #3460 ) ;
#7450 = EDGE_LOOP ( 'NONE', ( #16809, #20799, #21158, #15601 ) ) ;
#7451 = VERTEX_POINT ( 'NONE', #5163 ) ;
#7452 = CONTEXT_DEPENDENT_SHAPE_REPRESENTATION ( #10868, #1265 ) ;
#7453 = ORIENTED_EDGE ( 'NONE', *, *, #19171, .T. ) ;
#7454 = CARTESIAN_POINT ( 'NONE',  ( -23.85000000000000497, 15.03999999999999915, 27.00000000000000000 ) ) ;
#7455 = CARTESIAN_POINT ( 'NONE',  ( -5.871322893124554021, 8.081182679343978492, 9.906742014460235168 ) ) ;
#7456 = EDGE_LOOP ( 'NONE', ( #4824, #19447, #3933, #8312, #16229, #18370 ) ) ;
#7457 = AXIS2_PLACEMENT_3D ( 'NONE', #15305, #13240, #219 ) ;
#7458 = CIRCLE ( 'NONE', #21121, 0.9999999999999991118 ) ;
#7459 = CONICAL_SURFACE ( 'NONE', #21124, 4.249999999999993783, 1.029744258676653645 ) ;
#7460 = DIRECTION ( 'NONE',  ( -1.000000000000000000, 0.000000000000000000, 0.000000000000000000 ) ) ;
#7461 = AXIS2_PLACEMENT_3D ( 'NONE', #15905, #15636, #23061 ) ;
#7462 = EDGE_LOOP ( 'NONE', ( #9457, #10021, #6464, #9312 ) ) ;
#7463 = LINE ( 'NONE', #11128, #8233 ) ;
#7464 = CIRCLE ( 'NONE', #16885, 11.00000000000001066 ) ;
#7465 = CARTESIAN_POINT ( 'NONE',  ( 7.685661446562381371, -5.583959896777971110, 11.00674201446023304 ) ) ;
#7466 = CARTESIAN_POINT ( 'NONE',  ( 23.00000000000000000, -1.934484387512043435, 14.08058594723506474 ) ) ;
#7467 = CARTESIAN_POINT ( 'NONE',  ( 76.32931906745326955, -9.244463733058732095E-30, 5.000000000000007994 ) ) ;
#7468 = CARTESIAN_POINT ( 'NONE',  ( 74.00000000000001421, 7.491529369508391930E-15, 0.000000000000000000 ) ) ;
#7469 = EDGE_CURVE ( 'NONE', #3022, #978, #16824, .T. ) ;
#7470 = DIRECTION ( 'NONE',  ( 0.000000000000000000, -1.000000000000000000, 0.000000000000000000 ) ) ;
#7471 = ADVANCED_FACE ( 'NONE', ( #14545 ), #15666, .T. ) ;
#7472 = CARTESIAN_POINT ( 'NONE',  ( 68.76159002345582394, 5.000000000000015099, 0.000000000000000000 ) ) ;
#7473 = ORIENTED_EDGE ( 'NONE', *, *, #12163, .T. ) ;
#7474 = CARTESIAN_POINT ( 'NONE',  ( -8.680847955710813579, -2.820578480814258437, 5.733165578109188587 ) ) ;
#7475 = ORIENTED_EDGE ( 'NONE', *, *, #11379, .T. ) ;
#7476 = AXIS2_PLACEMENT_3D ( 'NONE', #8104, #2385, #11264 ) ;
#7477 = CIRCLE ( 'NONE', #20358, 1.999999999999997113 ) ;
#7478 = AXIS2_PLACEMENT_3D ( 'NONE', #8160, #13797, #2812 ) ;
#7479 = APPLICATION_PROTOCOL_DEFINITION ( 'draft international standard', 'automotive_design', 1998, #3234 ) ;
#7480 = AXIS2_PLACEMENT_3D ( 'NONE', #14364, #10919, #14606 ) ;
#7481 = CIRCLE ( 'NONE', #21143, 4.172000000000008590 ) ;
#7482 = ORIENTED_EDGE ( 'NONE', *, *, #5608, .T. ) ;
#7483 = ORIENTED_EDGE ( 'NONE', *, *, #15884, .F. ) ;
#7484 = CARTESIAN_POINT ( 'NONE',  ( 14.51962751333974389, 3.765689428759029234, 27.00000000000000000 ) ) ;
#7485 = CARTESIAN_POINT ( 'NONE',  ( 5.365059087799946447, -7.384370330706356178, -8.333165578109190008 ) ) ;
#7486 = VECTOR ( 'NONE', #13353, 1000.000000000000000 ) ;
#7487 = ORIENTED_EDGE ( 'NONE', *, *, #4913, .T. ) ;
#7488 = DIRECTION ( 'NONE',  ( 6.811450227741984732E-14, -1.000000000000000000, 0.000000000000000000 ) ) ;
#7489 = CARTESIAN_POINT ( 'NONE',  ( 33.99999999999998579, -4.000000000000013323, 10.49999999999999822 ) ) ;
#7490 = DIRECTION ( 'NONE',  ( -0.000000000000000000, -0.000000000000000000, -1.000000000000000000 ) ) ;
#7491 = CARTESIAN_POINT ( 'NONE',  ( 41.99999999999999289, 5.618459588085056979E-15, -9.499999999999987566 ) ) ;
#7492 = ORIENTED_EDGE ( 'NONE', *, *, #11217, .T. ) ;
#7493 = CARTESIAN_POINT ( 'NONE',  ( -34.02499999999999858, 29.50000000000000000, -3.000000000000000000 ) ) ;
#7494 = EDGE_CURVE ( 'NONE', #4993, #6097, #20180, .T. ) ;
#7495 = VERTEX_POINT ( 'NONE', #1044 ) ;
#7496 = AXIS2_PLACEMENT_3D ( 'NONE', #3113, #19599, #17627 ) ;
#7497 = CARTESIAN_POINT ( 'NONE',  ( 9.500000000000000000, 6.470877716354879437E-13, -8.059589141758143782 ) ) ;
#7498 = DIRECTION ( 'NONE',  ( 0.000000000000000000, 0.000000000000000000, 1.000000000000000000 ) ) ;
#7499 = VECTOR ( 'NONE', #22026, 1000.000000000000000 ) ;
#7500 = CARTESIAN_POINT ( 'NONE',  ( 0.000000000000000000, 0.000000000000000000, 27.00000000000000000 ) ) ;
#7501 = DIRECTION ( 'NONE',  ( -0.000000000000000000, -0.000000000000000000, 1.000000000000000000 ) ) ;
#7502 = VECTOR ( 'NONE', #12977, 1000.000000000000000 ) ;
#7503 = EDGE_CURVE ( 'NONE', #22892, #10927, #6325, .T. ) ;
#7504 = AXIS2_PLACEMENT_3D ( 'NONE', #18353, #12740, #1644 ) ;
#7505 = DIRECTION ( 'NONE',  ( -1.000000000000000000, 0.000000000000000000, 0.000000000000000000 ) ) ;
#7506 = ADVANCED_FACE ( 'NONE', ( #17870 ), #10209, .T. ) ;
#7507 = DIRECTION ( 'NONE',  ( -0.000000000000000000, -0.000000000000000000, -1.000000000000000000 ) ) ;
#7508 = ADVANCED_FACE ( 'NONE', ( #11223 ), #7445, .T. ) ;
#7509 = CIRCLE ( 'NONE', #5197, 0.6999999999999996225 ) ;
#7510 = DIRECTION ( 'NONE',  ( 0.000000000000000000, 1.000000000000000000, 0.000000000000000000 ) ) ;
#7511 = ORIENTED_EDGE ( 'NONE', *, *, #14788, .F. ) ;
#7512 = ORIENTED_EDGE ( 'NONE', *, *, #17118, .F. ) ;
#7513 = ORIENTED_EDGE ( 'NONE', *, *, #18592, .T. ) ;
#7514 = ORIENTED_EDGE ( 'NONE', *, *, #23632, .F. ) ;
#7515 =( NAMED_UNIT ( * ) SI_UNIT ( $, .STERADIAN. ) SOLID_ANGLE_UNIT ( ) );
#7516 = AXIS2_PLACEMENT_3D ( 'NONE', #17946, #8650, #10599 ) ;
#7517 = CARTESIAN_POINT ( 'NONE',  ( 0.6999999999999996225, 0.000000000000000000, 0.000000000000000000 ) ) ;
#7518 = CIRCLE ( 'NONE', #14159, 5.100000000000000533 ) ;
#7519 = AXIS2_PLACEMENT_3D ( 'NONE', #11870, #10028, #17487 ) ;
#7520 = VECTOR ( 'NONE', #23321, 999.9999999999998863 ) ;
#7521 = VECTOR ( 'NONE', #16622, 1000.000000000000000 ) ;
#7522 = CARTESIAN_POINT ( 'NONE',  ( 62.94340820527399671, 5.000000000000015099, 0.000000000000000000 ) ) ;
#7523 = DIRECTION ( 'NONE',  ( -1.000000000000000000, -2.600433232233976523E-16, -0.000000000000000000 ) ) ;
#7524 = CARTESIAN_POINT ( 'NONE',  ( -39.99999999999999289, 29.50000000000000000, 27.00000000000000000 ) ) ;
#7525 = AXIS2_PLACEMENT_3D ( 'NONE', #13724, #22638, #21173 ) ;
#7526 = EDGE_CURVE ( 'NONE', #7845, #11886, #22137, .T. ) ;
#7527 = ORIENTED_EDGE ( 'NONE', *, *, #19028, .T. ) ;
#7528 = CARTESIAN_POINT ( 'NONE',  ( 28.27483331787887622, 41.23752903419610050, 27.00000000000000000 ) ) ;
#7529 = DIRECTION ( 'NONE',  ( -1.000000000000000000, 0.000000000000000000, 0.000000000000000000 ) ) ;
#7530 = CARTESIAN_POINT ( 'NONE',  ( -10.00000000000000000, 0.000000000000000000, 0.000000000000000000 ) ) ;
#7531 = DIRECTION ( 'NONE',  ( 0.000000000000000000, -1.000000000000000000, 0.000000000000000000 ) ) ;
#7532 = CARTESIAN_POINT ( 'NONE',  ( -31.74999999999995737, 0.000000000000000000, 0.000000000000000000 ) ) ;
#7533 = EDGE_CURVE ( 'NONE', #22050, #20652, #3925, .T. ) ;
#7534 = ORIENTED_EDGE ( 'NONE', *, *, #11217, .F. ) ;
#7535 = CARTESIAN_POINT ( 'NONE',  ( 5.365059087798938364, 7.384370330707087149, -6.933165578109188765 ) ) ;
#7536 = EDGE_CURVE ( 'NONE', #5717, #13291, #19971, .T. ) ;
#7537 = AXIS2_PLACEMENT_3D ( 'NONE', #20641, #22711, #18806 ) ;
#7538 = DIRECTION ( 'NONE',  ( -1.000000000000000000, 0.000000000000000000, 0.000000000000000000 ) ) ;
#7539 = ORIENTED_EDGE ( 'NONE', *, *, #18738, .T. ) ;
#7540 = CARTESIAN_POINT ( 'NONE',  ( 0.000000000000000000, 0.000000000000000000, 12.50000000000000000 ) ) ;
#7541 = VERTEX_POINT ( 'NONE', #5409 ) ;
#7542 = DIRECTION ( 'NONE',  ( 1.000000000000000000, 0.000000000000000000, 0.000000000000000000 ) ) ;
#7543 = CIRCLE ( 'NONE', #6407, 1.000000000000000888 ) ;
#7544 = CIRCLE ( 'NONE', #5622, 5.000000000000007994 ) ;
#7545 = ORIENTED_EDGE ( 'NONE', *, *, #18701, .T. ) ;
#7546 = CARTESIAN_POINT ( 'NONE',  ( 82.72727272727273373, -4.172000000000000597, 0.000000000000000000 ) ) ;
#7547 = AXIS2_PLACEMENT_3D ( 'NONE', #23771, #9983, #18279 ) ;
#7548 = LINE ( 'NONE', #9498, #11894 ) ;
#7549 = CARTESIAN_POINT ( 'NONE',  ( -41.99999999999999289, 25.93535998569253920, 27.00000000000000000 ) ) ;
#7550 = DIRECTION ( 'NONE',  ( 0.000000000000000000, 0.000000000000000000, 1.000000000000000000 ) ) ;
#7551 = CIRCLE ( 'NONE', #17718, 12.73082370883259884 ) ;
#7552 = CARTESIAN_POINT ( 'NONE',  ( -9.499999999999790390, -3.086737114213257804, -7.159589141758144315 ) ) ;
#7553 = ORIENTED_EDGE ( 'NONE', *, *, #3348, .T. ) ;
#7554 = VECTOR ( 'NONE', #5129, 1000.000000000000000 ) ;
#7555 = CARTESIAN_POINT ( 'NONE',  ( 72.54545454545454675, -4.172000000000000597, 5.616230220889771312E-16 ) ) ;
#7556 = CARTESIAN_POINT ( 'NONE',  ( 9.500000000000000000, 6.470877716354879437E-13, 11.20674201446023410 ) ) ;
#7557 = ORIENTED_EDGE ( 'NONE', *, *, #17594, .T. ) ;
#7558 = CARTESIAN_POINT ( 'NONE',  ( -6.250000000000000888, 10.82531754730548279, 2.500000000000000000 ) ) ;
#7559 = AXIS2_PLACEMENT_3D ( 'NONE', #12934, #18099, #3448 ) ;
#7560 = CARTESIAN_POINT ( 'NONE',  ( -23.90000000000000213, 29.49999999999999645, 11.50000000000000000 ) ) ;
#7561 =( NAMED_UNIT ( * ) SI_UNIT ( $, .STERADIAN. ) SOLID_ANGLE_UNIT ( ) );
#7562 = DIRECTION ( 'NONE',  ( 0.000000000000000000, 0.000000000000000000, 1.000000000000000000 ) ) ;
#7563 = ADVANCED_FACE ( 'NONE', ( #18813 ), #165, .T. ) ;
#7564 = DIRECTION ( 'NONE',  ( 1.000000000000000000, 0.000000000000000000, 0.000000000000000000 ) ) ;
#7565 = CYLINDRICAL_SURFACE ( 'NONE', #18095, 9.500000000000000000 ) ;
#7566 = LINE ( 'NONE', #7687, #18829 ) ;
#7567 = ORIENTED_EDGE ( 'NONE', *, *, #10744, .T. ) ;
#7568 = CARTESIAN_POINT ( 'NONE',  ( -31.50000000000001421, 50.99999999999999289, 0.5000000000000004441 ) ) ;
#7569 = DIRECTION ( 'NONE',  ( 0.000000000000000000, 0.000000000000000000, 1.000000000000000000 ) ) ;
#7570 = CARTESIAN_POINT ( 'NONE',  ( -39.49999999999998579, 15.50000000000000000, 19.70000000000000284 ) ) ;
#7571 = VECTOR ( 'NONE', #21149, 1000.000000000000000 ) ;
#7572 = CARTESIAN_POINT ( 'NONE',  ( 29.00000000000000000, -29.50000000000000355, 11.00000000000000000 ) ) ;
#7573 = ORIENTED_EDGE ( 'NONE', *, *, #3792, .T. ) ;
#7574 = VECTOR ( 'NONE', #16750, 1000.000000000000000 ) ;
#7575 = ORIENTED_EDGE ( 'NONE', *, *, #18852, .T. ) ;
#7576 = VECTOR ( 'NONE', #22103, 1000.000000000000000 ) ;
#7577 = CONTEXT_DEPENDENT_SHAPE_REPRESENTATION ( #1403, #18736 ) ;
#7578 = VERTEX_POINT ( 'NONE', #5650 ) ;
#7579 = FACE_OUTER_BOUND ( 'NONE', #16775, .T. ) ;
#7580 = LINE ( 'NONE', #15029, #11068 ) ;
#7581 = EDGE_CURVE ( 'NONE', #1636, #3226, #1865, .T. ) ;
#7582 = AXIS2_PLACEMENT_3D ( 'NONE', #22680, #9484, #13040 ) ;
#7583 = AXIS2_PLACEMENT_3D ( 'NONE', #12287, #21809, #20108 ) ;
#7584 = DIRECTION ( 'NONE',  ( -1.000000000000000000, -1.224606353822377258E-16, -0.000000000000000000 ) ) ;
#7585 = ORIENTED_EDGE ( 'NONE', *, *, #11240, .F. ) ;
#7586 = ORIENTED_EDGE ( 'NONE', *, *, #22246, .F. ) ;
#7587 = ADVANCED_FACE ( 'NONE', ( #20541 ), #3211, .T. ) ;
#7588 = DIRECTION ( 'NONE',  ( 1.000000000000000000, 0.000000000000000000, 0.000000000000000000 ) ) ;
#7589 = ORIENTED_EDGE ( 'NONE', *, *, #6858, .T. ) ;
#7590 = EDGE_CURVE ( 'NONE', #23563, #16008, #4405, .T. ) ;
#7591 = ADVANCED_FACE ( 'NONE', ( #20404 ), #289, .T. ) ;
#7592 = CARTESIAN_POINT ( 'NONE',  ( 80.69295543108962931, 7.420530141404717394E-15, 0.000000000000000000 ) ) ;
#7593 = CARTESIAN_POINT ( 'NONE',  ( -39.99999999999999289, 15.50000000000000000, 19.70000000000000284 ) ) ;
#7594 = DIRECTION ( 'NONE',  ( -0.000000000000000000, -0.000000000000000000, 1.000000000000000000 ) ) ;
#7595 = CIRCLE ( 'NONE', #6849, 5.000000000000007994 ) ;
#7596 = CARTESIAN_POINT ( 'NONE',  ( -6.370271264241011523E-16, -12.39061695991708412, 7.750000000000000000 ) ) ;
#7597 = VERTEX_POINT ( 'NONE', #18461 ) ;
#7598 = VERTEX_POINT ( 'NONE', #15129 ) ;
#7599 = FACE_OUTER_BOUND ( 'NONE', #10219, .T. ) ;
#7600 = CYLINDRICAL_SURFACE ( 'NONE', #10643, 3.000000000000002665 ) ;
#7601 = ORIENTED_EDGE ( 'NONE', *, *, #984, .F. ) ;
#7602 = CONICAL_SURFACE ( 'NONE', #24001, 4.172000000000008590, 0.9599310885968742602 ) ;
#7603 = EDGE_LOOP ( 'NONE', ( #6945, #6466, #6591 ) ) ;
#7604 = CARTESIAN_POINT ( 'NONE',  ( -9.499999999999790390, -3.086737114213257804, 11.15958914175814520 ) ) ;
#7605 = ORIENTED_EDGE ( 'NONE', *, *, #23896, .T. ) ;
#7606 = PRODUCT_CONTEXT ( 'NONE', #11474, 'mechanical' ) ;
#7607 = EDGE_LOOP ( 'NONE', ( #4104, #14723, #19034, #17922 ) ) ;
#7608 = EDGE_LOOP ( 'NONE', ( #5527, #15535, #8115, #9225 ) ) ;
#7609 = LINE ( 'NONE', #2506, #7486 ) ;
#7610 = CARTESIAN_POINT ( 'NONE',  ( 7.022953521754877748, 5.102474405760673903, -10.83316557810919001 ) ) ;
#7611 = EDGE_CURVE ( 'NONE', #3844, #14068, #5944, .T. ) ;
#7612 = VECTOR ( 'NONE', #15062, 1000.000000000000000 ) ;
#7613 =( GEOMETRIC_REPRESENTATION_CONTEXT ( 3 ) GLOBAL_UNCERTAINTY_ASSIGNED_CONTEXT ( ( #8612 ) ) GLOBAL_UNIT_ASSIGNED_CONTEXT ( ( #22086, #8889, #15971 ) ) REPRESENTATION_CONTEXT ( 'NONE', 'WORKASPACE' ) );
#7614 = DIRECTION ( 'NONE',  ( 0.000000000000000000, -1.000000000000000000, 0.000000000000000000 ) ) ;
#7615 = CIRCLE ( 'NONE', #13889, 20.85000000000000853 ) ;
#7616 = EDGE_LOOP ( 'NONE', ( #6157, #18290, #11018, #1719 ) ) ;
#7617 = DIRECTION ( 'NONE',  ( 0.4828336235133042775, -0.8757121056631643752, 0.000000000000000000 ) ) ;
#7618 = CARTESIAN_POINT ( 'NONE',  ( 14.51962751333974211, -3.765689428759034563, -8.721787840009190163 ) ) ;
#7619 = CYLINDRICAL_SURFACE ( 'NONE', #19016, 1.500000000000001332 ) ;
#7620 = ADVANCED_FACE ( 'NONE', ( #13302 ), #20768, .T. ) ;
#7621 = PRODUCT_DEFINITION_SHAPE ( 'NONE', 'NONE',  #8989 ) ;
#7622 = EDGE_CURVE ( 'NONE', #5720, #11259, #493, .T. ) ;
#7623 = CARTESIAN_POINT ( 'NONE',  ( 18.50000000000000000, 2.265596578422603396E-15, 15.50000000000000000 ) ) ;
#7624 = ORIENTED_EDGE ( 'NONE', *, *, #5435, .T. ) ;
#7625 = CONICAL_SURFACE ( 'NONE', #8026, 5.025000000000002132, 0.7853981633974482790 ) ;
#7626 = DIRECTION ( 'NONE',  ( -1.000000000000000000, 0.000000000000000000, 0.000000000000000000 ) ) ;
#7627 = VERTEX_POINT ( 'NONE', #9051 ) ;
#7628 = CARTESIAN_POINT ( 'NONE',  ( -40.89823313241237912, 26.41789760203348081, 27.00000000000000000 ) ) ;
#7629 = CARTESIAN_POINT ( 'NONE',  ( 23.00000000000000000, 14.21257171757157245, 0.08908218613057176938 ) ) ;
#7630 = LINE ( 'NONE', #9230, #21954 ) ;
#7631 = DIRECTION ( 'NONE',  ( 1.000000000000000000, 0.000000000000000000, 0.000000000000000000 ) ) ;
#7632 = CARTESIAN_POINT ( 'NONE',  ( 6.699999999999999289, 0.000000000000000000, 0.000000000000000000 ) ) ;
#7633 = CARTESIAN_POINT ( 'NONE',  ( -8.680847955711007202, -5.923547351154968927E-13, -11.63316557810919072 ) ) ;
#7634 = CIRCLE ( 'NONE', #21303, 0.9999999999999994449 ) ;
#7635 = AXIS2_PLACEMENT_3D ( 'NONE', #9822, #22791, #17157 ) ;
#7636 = ORIENTED_EDGE ( 'NONE', *, *, #8035, .F. ) ;
#7637 = CONICAL_SURFACE ( 'NONE', #24016, 7.999999999999986677, 0.7853981633974473908 ) ;
#7638 = ORIENTED_EDGE ( 'NONE', *, *, #15134, .T. ) ;
#7639 = ORIENTED_EDGE ( 'NONE', *, *, #16998, .F. ) ;
#7640 = VERTEX_POINT ( 'NONE', #22494 ) ;
#7641 = CIRCLE ( 'NONE', #22478, 8.000000000000000000 ) ;
#7642 = ORIENTED_EDGE ( 'NONE', *, *, #10488, .T. ) ;
#7643 = CARTESIAN_POINT ( 'NONE',  ( 9.500000000000000000, 6.470877716354879437E-13, 10.05958914175814378 ) ) ;
#7644 = UNCERTAINTY_MEASURE_WITH_UNIT (LENGTH_MEASURE( 1.000000000000000082E-05 ), #3554, 'distance_accuracy_value', 'NONE');
#7645 = ADVANCED_FACE ( 'NONE', ( #13186 ), #11330, .F. ) ;
#7646 = DIRECTION ( 'NONE',  ( 0.000000000000000000, 1.000000000000000000, 0.000000000000000000 ) ) ;
#7647 = CARTESIAN_POINT ( 'NONE',  ( -2.999999999999996447, 8.485281374238571317, 98.99999999999998579 ) ) ;
#7648 = CARTESIAN_POINT ( 'NONE',  ( -14.51962751333974033, -3.765689428759031010, -27.00000000000000000 ) ) ;
#7649 = EDGE_CURVE ( 'NONE', #4813, #8141, #17158, .T. ) ;
#7650 = ADVANCED_FACE ( 'NONE', ( #18082 ), #3075, .T. ) ;
#7651 = CIRCLE ( 'NONE', #21322, 1.500000000000001332 ) ;
#7652 = ORIENTED_EDGE ( 'NONE', *, *, #18189, .T. ) ;
#7653 = DIRECTION ( 'NONE',  ( -1.000000000000000000, 0.000000000000000000, 0.000000000000000000 ) ) ;
#7654 = ORIENTED_EDGE ( 'NONE', *, *, #8377, .T. ) ;
#7655 = DIRECTION ( 'NONE',  ( 1.000000000000000000, 0.000000000000000000, 0.000000000000000000 ) ) ;
#7656 = DIRECTION ( 'NONE',  ( -0.000000000000000000, -0.000000000000000000, 1.000000000000000000 ) ) ;
#7657 = FACE_OUTER_BOUND ( 'NONE', #3074, .T. ) ;
#7658 = CARTESIAN_POINT ( 'NONE',  ( -16.68617496892350260, 7.233372502334340481, 6.175747996014763430 ) ) ;
#7659 = CARTESIAN_POINT ( 'NONE',  ( 0.000000000000000000, 0.000000000000000000, 0.000000000000000000 ) ) ;
#7660 = EDGE_LOOP ( 'NONE', ( #11959, #22115, #18321, #19417, #20002 ) ) ;
#7661 = CARTESIAN_POINT ( 'NONE',  ( 6.222797240145152671E-13, -9.127583699786111282, -6.133165578109188942 ) ) ;
#7662 = ORIENTED_EDGE ( 'NONE', *, *, #626, .F. ) ;
#7663 = CARTESIAN_POINT ( 'NONE',  ( 20.85000000000000497, 15.03999999999999737, 2.200000000000000178 ) ) ;
#7664 = ORIENTED_EDGE ( 'NONE', *, *, #14769, .T. ) ;
#7665 = CARTESIAN_POINT ( 'NONE',  ( -9.499999999999799272, -3.086737114213243593, -9.159589141758143427 ) ) ;
#7666 = ORIENTED_EDGE ( 'NONE', *, *, #18003, .T. ) ;
#7667 = DIRECTION ( 'NONE',  ( 0.000000000000000000, -1.000000000000000000, 0.000000000000000000 ) ) ;
#7668 = CARTESIAN_POINT ( 'NONE',  ( 82.72727272727273373, 7.491529369508391930E-15, 0.000000000000000000 ) ) ;
#7669 = EDGE_CURVE ( 'NONE', #2457, #13300, #1376, .T. ) ;
#7670 = FACE_OUTER_BOUND ( 'NONE', #15966, .T. ) ;
#7671 = LINE ( 'NONE', #6105, #9160 ) ;
#7672 = DIRECTION ( 'NONE',  ( -1.000000000000000000, -0.000000000000000000, -0.000000000000000000 ) ) ;
#7673 = EDGE_CURVE ( 'NONE', #22991, #16629, #6616, .T. ) ;
#7674 = EDGE_CURVE ( 'NONE', #16347, #8203, #4792, .T. ) ;
#7675 = CARTESIAN_POINT ( 'NONE',  ( -7.685661446561619314, -5.583959896779019161, -7.259589141758143960 ) ) ;
#7676 = ORIENTED_EDGE ( 'NONE', *, *, #9515, .F. ) ;
#7677 = FACE_OUTER_BOUND ( 'NONE', #7836, .T. ) ;
#7678 = EDGE_LOOP ( 'NONE', ( #19815, #3567, #7482, #5002 ) ) ;
#7679 = DIRECTION ( 'NONE',  ( -1.000000000000000000, 0.000000000000000000, 0.000000000000000000 ) ) ;
#7680 = CIRCLE ( 'NONE', #11192, 2.024999999999999911 ) ;
#7681 = CARTESIAN_POINT ( 'NONE',  ( 0.3931297258116509541, 8.993512908210947288, 78.01929305477952425 ) ) ;
#7682 = DIRECTION ( 'NONE',  ( 0.000000000000000000, 0.000000000000000000, -1.000000000000000000 ) ) ;
#7683 = CARTESIAN_POINT ( 'NONE',  ( -42.00000000000000000, 25.22443390181683043, -1.500000000000000000 ) ) ;
#7684 = DIRECTION ( 'NONE',  ( -0.000000000000000000, -0.000000000000000000, 1.000000000000000000 ) ) ;
#7685 = CARTESIAN_POINT ( 'NONE',  ( -9.500000000000216716, 3.086737114211953514, -8.106742014460232681 ) ) ;
#7686 = CARTESIAN_POINT ( 'NONE',  ( 80.39795365981946418, 7.562528597612068045E-15, 0.000000000000000000 ) ) ;
#7687 = CARTESIAN_POINT ( 'NONE',  ( 44.99999999999998579, 50.99999999999992184, 12.50000000000000000 ) ) ;
#7688 = ORIENTED_EDGE ( 'NONE', *, *, #22699, .F. ) ;
#7689 = DIRECTION ( 'NONE',  ( -0.000000000000000000, 1.000000000000000000, -0.000000000000000000 ) ) ;
#7690 = PRODUCT_DEFINITION_SHAPE ( 'NONE', 'NONE',  #24122 ) ;
#7691 = DIRECTION ( 'NONE',  ( -0.000000000000000000, 0.000000000000000000, 1.000000000000000000 ) ) ;
#7692 = CARTESIAN_POINT ( 'NONE',  ( -36.00000000000001421, 50.99999999999999289, 0.5000000000000000000 ) ) ;
#7693 = CARTESIAN_POINT ( 'NONE',  ( 9.500000000000000000, 1.163414459189985485E-15, 12.50000000000000000 ) ) ;
#7694 = EDGE_CURVE ( 'NONE', #21516, #1993, #2037, .T. ) ;
#7695 = CARTESIAN_POINT ( 'NONE',  ( 81.27272727272728048, 7.491529369508391930E-15, 0.000000000000000000 ) ) ;
#7696 = VERTEX_POINT ( 'NONE', #8796 ) ;
#7697 = AXIS2_PLACEMENT_3D ( 'NONE', #2381, #18739, #2147 ) ;
#7698 = ORIENTED_EDGE ( 'NONE', *, *, #7533, .F. ) ;
#7699 = ORIENTED_EDGE ( 'NONE', *, *, #6519, .T. ) ;
#7700 = VERTEX_POINT ( 'NONE', #16241 ) ;
#7701 = DIRECTION ( 'NONE',  ( 0.000000000000000000, 0.000000000000000000, 1.000000000000000000 ) ) ;
#7702 = EDGE_CURVE ( 'NONE', #23460, #13664, #17844, .T. ) ;
#7703 = EDGE_CURVE ( 'NONE', #5301, #678, #18791, .T. ) ;
#7704 = CARTESIAN_POINT ( 'NONE',  ( 40.23082370883258818, -29.49999999999999645, -3.000000000000000000 ) ) ;
#7705 = ORIENTED_EDGE ( 'NONE', *, *, #2100, .F. ) ;
#7706 = VERTEX_POINT ( 'NONE', #10734 ) ;
#7707 = DIRECTION ( 'NONE',  ( -0.000000000000000000, -0.000000000000000000, -1.000000000000000000 ) ) ;
#7708 = EDGE_LOOP ( 'NONE', ( #17079, #3434, #13253, #15622 ) ) ;
#7709 = CYLINDRICAL_SURFACE ( 'NONE', #6555, 5.100000000000000533 ) ;
#7710 = ORIENTED_EDGE ( 'NONE', *, *, #16151, .T. ) ;
#7711 = FACE_BOUND ( 'NONE', #11907, .T. ) ;
#7712 = CARTESIAN_POINT ( 'NONE',  ( 0.000000000000000000, -7.033831428820064069, -16.43291941292179104 ) ) ;
#7713 = CARTESIAN_POINT ( 'NONE',  ( 23.00000000000000000, 12.02595010061954284, 13.22467954916291433 ) ) ;
#7714 = AXIS2_PLACEMENT_3D ( 'NONE', #11696, #22844, #15119 ) ;
#7715 = DIRECTION ( 'NONE',  ( -0.5735764363510519326, 0.8191520442889876907, 1.003171929053519816E-16 ) ) ;
#7716 = ORIENTED_EDGE ( 'NONE', *, *, #16437, .T. ) ;
#7717 = DIRECTION ( 'NONE',  ( 0.7052211081716905916, 0.7089874389501501506, -0.000000000000000000 ) ) ;
#7718 = PLANE ( 'NONE',  #1305 ) ;
#7719 = EDGE_CURVE ( 'NONE', #1654, #7244, #4816, .T. ) ;
#7720 = DIRECTION ( 'NONE',  ( -1.000000000000000000, -0.000000000000000000, 0.000000000000000000 ) ) ;
#7721 = ORIENTED_EDGE ( 'NONE', *, *, #993, .F. ) ;
#7722 = EDGE_LOOP ( 'NONE', ( #22965, #15048, #20764, #17392 ) ) ;
#7723 = CARTESIAN_POINT ( 'NONE',  ( 2.682529543899157876, 8.255977015246598327, 5.033165578109189298 ) ) ;
#7724 = ORIENTED_EDGE ( 'NONE', *, *, #20306, .F. ) ;
#7725 = EDGE_CURVE ( 'NONE', #23989, #19319, #9066, .T. ) ;
#7726 = CLOSED_SHELL ( 'NONE', ( #8183, #10565, #16969, #17991, #10446, #5022, #3831, #14949, #10910, #14966, #16007, #20444, #13884, #22626, #1442, #1212, #8120, #1837, #3143, #9060, #23522, #715, #3115, #1580, #19648, #22698, #5822, #8702, #2163, #15084, #24013, #10072, #3323, #9680, #15557, #12002, #22834, #1875, #3411, #16758, #18631, #19899, #18375, #2005, #11973, #14247, #9371, #6309, #7937, #14915, #22036, #15182, #18726, #12168, #7620, #8696, #7283, #7415, #6406, #1475, #6151, #16034, #17204, #7228, #22944, #23247, #23835, #3674, #2462, #23226, #3808, #19298, #18188, #17242, #8499, #21649, #5224, #8997, #6934, #14546, #20439, #10235, #11190, #4706, #1410, #12960, #21496, #9274, #20412, #14682, #905, #23574, #21644, #16496, #14169, #22300, #19612, #10626 ) ) ;
#7727 = DIRECTION ( 'NONE',  ( -1.000000000000000000, -0.000000000000000000, -0.000000000000000000 ) ) ;
#7728 = VERTEX_POINT ( 'NONE', #14509 ) ;
#7729 = VERTEX_POINT ( 'NONE', #4670 ) ;
#7730 = EDGE_CURVE ( 'NONE', #1315, #6030, #3625, .T. ) ;
#7731 = DIRECTION ( 'NONE',  ( 0.000000000000000000, -1.000000000000000000, 0.000000000000000000 ) ) ;
#7732 = CARTESIAN_POINT ( 'NONE',  ( 8.680847955710813579, 2.820578480814259326, -10.73316557810918503 ) ) ;
#7733 = EDGE_CURVE ( 'NONE', #5307, #4702, #20376, .T. ) ;
#7734 = DIRECTION ( 'NONE',  ( 0.5801326495544486539, 9.975017754987290696E-17, 0.8145220125453549453 ) ) ;
#7735 = ORIENTED_EDGE ( 'NONE', *, *, #12229, .T. ) ;
#7736 = DIRECTION ( 'NONE',  ( 0.000000000000000000, -1.000000000000000000, 0.000000000000000000 ) ) ;
#7737 = DIRECTION ( 'NONE',  ( -1.000000000000000000, 0.000000000000000000, 0.000000000000000000 ) ) ;
#7738 = DIRECTION ( 'NONE',  ( -0.000000000000000000, -0.000000000000000000, -1.000000000000000000 ) ) ;
#7739 = DIRECTION ( 'NONE',  ( 0.000000000000000000, 0.000000000000000000, 1.000000000000000000 ) ) ;
#7740 = CARTESIAN_POINT ( 'NONE',  ( -23.85000000000000497, 15.03999999999999915, 25.00000000000000000 ) ) ;
#7741 = EDGE_LOOP ( 'NONE', ( #7864, #4787 ) ) ;
#7742 = DIRECTION ( 'NONE',  ( 1.000000000000000000, 0.000000000000000000, -0.000000000000000000 ) ) ;
#7743 = CARTESIAN_POINT ( 'NONE',  ( 0.000000000000000000, 0.000000000000000000, 0.000000000000000000 ) ) ;
#7744 = ORIENTED_EDGE ( 'NONE', *, *, #12371, .F. ) ;
#7745 = CARTESIAN_POINT ( 'NONE',  ( -24.75000000000000000, 29.50000000000000000, -2.224999999999995204 ) ) ;
#7746 = CARTESIAN_POINT ( 'NONE',  ( 9.499999999999790390, 3.086737114213260025, -8.159589141758143427 ) ) ;
#7747 = DIRECTION ( 'NONE',  ( -0.000000000000000000, -0.000000000000000000, -1.000000000000000000 ) ) ;
#7748 = DIRECTION ( 'NONE',  ( -0.000000000000000000, -0.000000000000000000, 1.000000000000000000 ) ) ;
#7749 = DIRECTION ( 'NONE',  ( 1.000000000000000000, 0.000000000000000000, 0.000000000000000000 ) ) ;
#7750 = CARTESIAN_POINT ( 'NONE',  ( -44.00000000000001421, 50.99999999999999289, 0.000000000000000000 ) ) ;
#7751 = ADVANCED_FACE ( 'NONE', ( #22222 ), #12185, .T. ) ;
#7752 = CARTESIAN_POINT ( 'NONE',  ( 2.570122167802765922, 0.000000000000000000, 0.000000000000000000 ) ) ;
#7753 = EDGE_LOOP ( 'NONE', ( #6895, #3265, #17166, #13135, #17448, #2724 ) ) ;
#7754 = ORIENTED_EDGE ( 'NONE', *, *, #14628, .T. ) ;
#7755 = EDGE_CURVE ( 'NONE', #10996, #10096, #5962, .T. ) ;
#7756 = ORIENTED_EDGE ( 'NONE', *, *, #11463, .T. ) ;
#7757 = ORIENTED_EDGE ( 'NONE', *, *, #12262, .T. ) ;
#7758 = LINE ( 'NONE', #11176, #2578 ) ;
#7759 = CIRCLE ( 'NONE', #17120, 4.499999999999997335 ) ;
#7760 = CIRCLE ( 'NONE', #386, 5.000000000000007994 ) ;
#7761 = CARTESIAN_POINT ( 'NONE',  ( 6.976272796952942556, -5.349986750954705883, 12.50000000000000000 ) ) ;
#7762 = DIRECTION ( 'NONE',  ( -1.000000000000000000, -0.000000000000000000, -0.000000000000000000 ) ) ;
#7763 = DIRECTION ( 'NONE',  ( 0.000000000000000000, -1.000000000000000000, 0.000000000000000000 ) ) ;
#7764 = FACE_OUTER_BOUND ( 'NONE', #9396, .T. ) ;
#7765 = CARTESIAN_POINT ( 'NONE',  ( 40.00000000000000000, -29.50000000000000000, 27.00000000000000000 ) ) ;
#7766 = DIRECTION ( 'NONE',  ( 1.000000000000000000, 0.000000000000000000, 0.000000000000000000 ) ) ;
#7767 = CARTESIAN_POINT ( 'NONE',  ( 0.000000000000000000, -45.00000000000000000, -8.673617379884035472E-16 ) ) ;
#7768 = DIRECTION ( 'NONE',  ( -0.000000000000000000, -0.000000000000000000, -1.000000000000000000 ) ) ;
#7769 = CARTESIAN_POINT ( 'NONE',  ( -17.05196227081077964, 8.053793831531468328, -5.044162359773903148 ) ) ;
#7770 = CARTESIAN_POINT ( 'NONE',  ( -31.74999999999995737, 0.000000000000000000, 0.000000000000000000 ) ) ;
#7771 = ORIENTED_EDGE ( 'NONE', *, *, #18379, .F. ) ;
#7772 = DIRECTION ( 'NONE',  ( -1.000000000000000000, 0.000000000000000000, 0.000000000000000000 ) ) ;
#7773 = EDGE_LOOP ( 'NONE', ( #2399, #13908, #9360, #17725 ) ) ;
#7774 = ORIENTED_EDGE ( 'NONE', *, *, #5985, .T. ) ;
#7775 = VECTOR ( 'NONE', #8653, 1000.000000000000000 ) ;
#7776 = CARTESIAN_POINT ( 'NONE',  ( 5.871322893124553133, -8.081182679343980269, 9.759589141758143072 ) ) ;
#7777 = EDGE_CURVE ( 'NONE', #2350, #20120, #7321, .T. ) ;
#7778 = EDGE_CURVE ( 'NONE', #17766, #21563, #3227, .T. ) ;
#7779 = ORIENTED_EDGE ( 'NONE', *, *, #11239, .F. ) ;
#7780 =( LENGTH_UNIT ( ) NAMED_UNIT ( * ) SI_UNIT ( .MILLI., .METRE. ) );
#7781 = CARTESIAN_POINT ( 'NONE',  ( 0.000000000000000000, 0.000000000000000000, 0.4999999999999995559 ) ) ;
#7782 = DIRECTION ( 'NONE',  ( -0.000000000000000000, 0.000000000000000000, 1.000000000000000000 ) ) ;
#7783 = CARTESIAN_POINT ( 'NONE',  ( -41.99999999999999289, -25.93535998569255341, 27.00000000000000000 ) ) ;
#7784 = DIRECTION ( 'NONE',  ( 0.000000000000000000, 1.000000000000000000, 0.000000000000000000 ) ) ;
#7785 = CARTESIAN_POINT ( 'NONE',  ( 10.00000000000000888, 15.50000000000000000, -2.999999999999999112 ) ) ;
#7786 = DIRECTION ( 'NONE',  ( 1.000000000000000000, 0.000000000000000000, -0.000000000000000000 ) ) ;
#7787 = ORIENTED_EDGE ( 'NONE', *, *, #5918, .T. ) ;
#7788 = VECTOR ( 'NONE', #2096, 1000.000000000000000 ) ;
#7789 = VERTEX_POINT ( 'NONE', #22340 ) ;
#7790 = CARTESIAN_POINT ( 'NONE',  ( -8.999999999999998224, 1.132798289211301501E-15, -12.50000000000000000 ) ) ;
#7791 = CARTESIAN_POINT ( 'NONE',  ( 2.257862244182143208, 8.713325772094773214, 79.01511099006255279 ) ) ;
#7792 = CARTESIAN_POINT ( 'NONE',  ( 0.000000000000000000, 0.000000000000000000, -3.499999999999999556 ) ) ;
#7793 = EDGE_CURVE ( 'NONE', #7700, #21154, #9837, .T. ) ;
#7794 = CYLINDRICAL_SURFACE ( 'NONE', #10510, 1.000000000000000888 ) ;
#7795 = CARTESIAN_POINT ( 'NONE',  ( -23.89999999999999858, -29.50000000000001066, 27.00000000000000000 ) ) ;
#7796 = FACE_OUTER_BOUND ( 'NONE', #8853, .T. ) ;
#7797 = DIRECTION ( 'NONE',  ( 0.000000000000000000, 0.000000000000000000, -1.000000000000000000 ) ) ;
#7798 = EDGE_CURVE ( 'NONE', #9249, #14555, #18562, .T. ) ;
#7799 = CARTESIAN_POINT ( 'NONE',  ( 2.935661446562616295, -9.035036904803758873, -6.806742014460233747 ) ) ;
#7800 = ORIENTED_EDGE ( 'NONE', *, *, #14252, .T. ) ;
#7801 = FACE_OUTER_BOUND ( 'NONE', #21153, .T. ) ;
#7802 = CARTESIAN_POINT ( 'NONE',  ( 8.680847955711007202, 5.912916378492122225E-13, 10.63316557810918894 ) ) ;
#7803 = ADVANCED_FACE ( 'NONE', ( #14758 ), #2051, .T. ) ;
#7804 = EDGE_CURVE ( 'NONE', #22047, #18868, #23103, .T. ) ;
#7805 = EDGE_CURVE ( 'NONE', #18693, #3802, #20447, .T. ) ;
#7806 = DIRECTION ( 'NONE',  ( 0.000000000000000000, 0.000000000000000000, -1.000000000000000000 ) ) ;
#7807 = DIRECTION ( 'NONE',  ( -0.7052211081716904806, 0.7089874389501500396, 0.000000000000000000 ) ) ;
#7808 = CIRCLE ( 'NONE', #21084, 1.000000000000000888 ) ;
#7809 = ORIENTED_EDGE ( 'NONE', *, *, #19855, .T. ) ;
#7810 = VECTOR ( 'NONE', #14828, 1000.000000000000000 ) ;
#7811 = DIRECTION ( 'NONE',  ( 0.000000000000000000, 0.000000000000000000, 1.000000000000000000 ) ) ;
#7812 = CARTESIAN_POINT ( 'NONE',  ( -5.871322893123450015, -8.081182679344781405, -10.50674201446023304 ) ) ;
#7813 = ORIENTED_EDGE ( 'NONE', *, *, #13417, .T. ) ;
#7814 = ORIENTED_EDGE ( 'NONE', *, *, #22214, .T. ) ;
#7815 = LINE ( 'NONE', #4199, #22885 ) ;
#7816 = ORIENTED_EDGE ( 'NONE', *, *, #19144, .F. ) ;
#7817 = ADVANCED_FACE ( 'NONE', ( #13158 ), #22466, .T. ) ;
#7818 = AXIS2_PLACEMENT_3D ( 'NONE', #8289, #6486, #23203 ) ;
#7819 = VECTOR ( 'NONE', #17395, 1000.000000000000000 ) ;
#7820 = ORIENTED_EDGE ( 'NONE', *, *, #12455, .F. ) ;
#7821 = CARTESIAN_POINT ( 'NONE',  ( -31.10231664966676135, 45.36128193761570770, -27.00000000000000000 ) ) ;
#7822 = CARTESIAN_POINT ( 'NONE',  ( 69.05659179472598908, 5.000000000000007105, 6.123233995736765296E-16 ) ) ;
#7823 = CIRCLE ( 'NONE', #11331, 4.999999999999997335 ) ;
#7824 = DIRECTION ( 'NONE',  ( 1.000000000000000000, 0.000000000000000000, 0.000000000000000000 ) ) ;
#7825 = LINE ( 'NONE', #6029, #5255 ) ;
#7826 = ORIENTED_EDGE ( 'NONE', *, *, #6276, .T. ) ;
#7827 = CARTESIAN_POINT ( 'NONE',  ( 3.890962118697714531E-15, 15.50000000000000000, 7.700000000000001954 ) ) ;
#7828 = DIRECTION ( 'NONE',  ( 0.000000000000000000, 0.000000000000000000, 1.000000000000000000 ) ) ;
#7829 = EDGE_CURVE ( 'NONE', #13833, #4922, #7203, .T. ) ;
#7830 = DIRECTION ( 'NONE',  ( 1.000000000000000000, 0.000000000000000000, -0.000000000000000000 ) ) ;
#7831 = VERTEX_POINT ( 'NONE', #3432 ) ;
#7832 = EDGE_CURVE ( 'NONE', #666, #15840, #7885, .T. ) ;
#7833 = EDGE_LOOP ( 'NONE', ( #15436, #11847, #22310, #23853 ) ) ;
#7834 = CARTESIAN_POINT ( 'NONE',  ( 7.685661446562381371, -5.583959896777971110, 11.85958914175814449 ) ) ;
#7835 = ORIENTED_EDGE ( 'NONE', *, *, #10039, .T. ) ;
#7836 = EDGE_LOOP ( 'NONE', ( #23774, #4263, #10204, #8524, #8973, #5048 ) ) ;
#7837 = FACE_OUTER_BOUND ( 'NONE', #7976, .T. ) ;
#7838 = AXIS2_PLACEMENT_3D ( 'NONE', #10342, #6206, #13767 ) ;
#7839 = VERTEX_POINT ( 'NONE', #9017 ) ;
#7840 = ORIENTED_EDGE ( 'NONE', *, *, #17154, .F. ) ;
#7841 = AXIS2_PLACEMENT_3D ( 'NONE', #22188, #7747, #5576 ) ;
#7842 = DIRECTION ( 'NONE',  ( -0.000000000000000000, -0.000000000000000000, -1.000000000000000000 ) ) ;
#7843 = DIRECTION ( 'NONE',  ( 1.000000000000000000, 4.163336342344333082E-15, 0.000000000000000000 ) ) ;
#7844 = CONICAL_SURFACE ( 'NONE', #7461, 4.172000000000008590, 0.9599310885968742602 ) ;
#7845 = VERTEX_POINT ( 'NONE', #5385 ) ;
#7846 = DIRECTION ( 'NONE',  ( -0.000000000000000000, -0.000000000000000000, 1.000000000000000000 ) ) ;
#7847 = DIRECTION ( 'NONE',  ( -1.000000000000000000, -1.224606353822377258E-16, -0.000000000000000000 ) ) ;
#7848 = CARTESIAN_POINT ( 'NONE',  ( -18.49999999999999645, -15.23000000000000220, 27.00000000000000000 ) ) ;
#7849 = DIRECTION ( 'NONE',  ( -1.000000000000000000, -0.000000000000000000, -0.000000000000000000 ) ) ;
#7850 = ORIENTED_EDGE ( 'NONE', *, *, #16126, .T. ) ;
#7851 = DIRECTION ( 'NONE',  ( 0.000000000000000000, 0.000000000000000000, 1.000000000000000000 ) ) ;
#7852 = ORIENTED_EDGE ( 'NONE', *, *, #16361, .F. ) ;
#7853 = CARTESIAN_POINT ( 'NONE',  ( 7.685661446562381371, -5.583959896777971110, -7.859589141758143604 ) ) ;
#7854 = DIRECTION ( 'NONE',  ( 1.000000000000000000, 0.000000000000000000, 0.000000000000000000 ) ) ;
#7855 = DIRECTION ( 'NONE',  ( 0.000000000000000000, 0.000000000000000000, 1.000000000000000000 ) ) ;
#7856 = AXIS2_PLACEMENT_3D ( 'NONE', #5344, #23537, #6816 ) ;
#7857 = DIRECTION ( 'NONE',  ( 3.469446951953610639E-15, -1.000000000000000000, 0.000000000000000000 ) ) ;
#7858 = CARTESIAN_POINT ( 'NONE',  ( -41.73082370883257397, -27.62204025492845361, 0.000000000000000000 ) ) ;
#7859 = CIRCLE ( 'NONE', #6338, 17.87500000001787726 ) ;
#7860 = EDGE_CURVE ( 'NONE', #23753, #2253, #19619, .T. ) ;
#7861 = VECTOR ( 'NONE', #16576, 1000.000000000000000 ) ;
#7862 = CIRCLE ( 'NONE', #21541, 10.00000000000000888 ) ;
#7863 = FACE_OUTER_BOUND ( 'NONE', #17341, .T. ) ;
#7864 = ORIENTED_EDGE ( 'NONE', *, *, #1211, .F. ) ;
#7865 = ORIENTED_EDGE ( 'NONE', *, *, #20051, .F. ) ;
#7866 = AXIS2_PLACEMENT_3D ( 'NONE', #7107, #6990, #21654 ) ;
#7867 = ORIENTED_EDGE ( 'NONE', *, *, #16738, .F. ) ;
#7868 = DIRECTION ( 'NONE',  ( 0.000000000000000000, 0.000000000000000000, 1.000000000000000000 ) ) ;
#7869 = EDGE_LOOP ( 'NONE', ( #16866, #23521, #14037, #6581 ) ) ;
#7870 = LINE ( 'NONE', #13254, #2526 ) ;
#7871 = DIRECTION ( 'NONE',  ( -0.000000000000000000, -0.000000000000000000, -1.000000000000000000 ) ) ;
#7872 = UNCERTAINTY_MEASURE_WITH_UNIT (LENGTH_MEASURE( 1.000000000000000082E-05 ), #3623, 'distance_accuracy_value', 'NONE');
#7873 = CARTESIAN_POINT ( 'NONE',  ( 9.500000000000209610, -3.086737114211962396, -11.10674201446023446 ) ) ;
#7875 = AXIS2_PLACEMENT_3D ( 'NONE', #23039, #2178, #20718 ) ;
#7874 = DIRECTION ( 'NONE',  ( 1.000000000000000000, 0.000000000000000000, 0.000000000000000000 ) ) ;
#7876 = CARTESIAN_POINT ( 'NONE',  ( 9.500000000000200728, -3.086737114211976607, 7.106742014460232681 ) ) ;
#7877 = DIRECTION ( 'NONE',  ( -1.000000000000000000, 0.000000000000000000, 0.000000000000000000 ) ) ;
#7878 = AXIS2_PLACEMENT_3D ( 'NONE', #5124, #22211, #14636 ) ;
#7879 = ADVANCED_FACE ( 'NONE', ( #14647 ), #901, .T. ) ;
#7880 = AXIS2_PLACEMENT_3D ( 'NONE', #11753, #17504, #19229 ) ;
#7881 = AXIS2_PLACEMENT_3D ( 'NONE', #22393, #7956, #9910 ) ;
#7882 = ORIENTED_EDGE ( 'NONE', *, *, #3030, .T. ) ;
#7883 = VECTOR ( 'NONE', #9380, 1000.000000000000000 ) ;
#7884 = CARTESIAN_POINT ( 'NONE',  ( 23.90000000000000568, -29.50000000000000355, 11.50000000000000000 ) ) ;
#7885 = CIRCLE ( 'NONE', #8279, 5.099999999999996980 ) ;
#7886 = EDGE_CURVE ( 'NONE', #8068, #20194, #17253, .T. ) ;
#7887 = DIRECTION ( 'NONE',  ( 0.000000000000000000, 0.000000000000000000, -1.000000000000000000 ) ) ;
#7888 = ORIENTED_EDGE ( 'NONE', *, *, #13051, .T. ) ;
#7889 = CARTESIAN_POINT ( 'NONE',  ( 63.81818181818181301, -4.172000000000000597, 0.000000000000000000 ) ) ;
#7890 = AXIS2_PLACEMENT_3D ( 'NONE', #2373, #9790, #17256 ) ;
#7891 = CARTESIAN_POINT ( 'NONE',  ( -14.51962751333974211, 3.765689428759028790, -8.721787840009202597 ) ) ;
#7892 = EDGE_CURVE ( 'NONE', #9833, #8545, #12565, .T. ) ;
#7893 = ADVANCED_FACE ( 'NONE', ( #19040 ), #17066, .F. ) ;
#7894 = CARTESIAN_POINT ( 'NONE',  ( 7.685661446562381371, -5.583959896777971110, 5.006742014460233037 ) ) ;
#7895 = CARTESIAN_POINT ( 'NONE',  ( 2.682529543899157876, 8.255977015246598327, -7.033165578109189298 ) ) ;
#7896 = ORIENTED_EDGE ( 'NONE', *, *, #13025, .F. ) ;
#7897 = EDGE_LOOP ( 'NONE', ( #15539, #13316, #23120, #8827 ) ) ;
#7898 = AXIS2_PLACEMENT_3D ( 'NONE', #14093, #10054, #2642 ) ;
#7899 = CARTESIAN_POINT ( 'NONE',  ( 7.685661446562381371, -5.583959896777971110, 9.859589141758144493 ) ) ;
#7900 = AXIS2_PLACEMENT_3D ( 'NONE', #12881, #7392, #14726 ) ;
#7901 = AXIS2_PLACEMENT_3D ( 'NONE', #4822, #2983, #21284 ) ;
#7902 = EDGE_LOOP ( 'NONE', ( #10845, #17501, #11988, #7639 ) ) ;
#7903 = AXIS2_PLACEMENT_3D ( 'NONE', #16290, #5189, #1542 ) ;
#7904 = CARTESIAN_POINT ( 'NONE',  ( 23.00000000000000000, 5.823083658124710738, 12.96521604808350503 ) ) ;
#7905 = CARTESIAN_POINT ( 'NONE',  ( 70.21613547800127719, 7.562528597612068045E-15, 0.000000000000000000 ) ) ;
#7906 = AXIS2_PLACEMENT_3D ( 'NONE', #3456, #5159, #22010 ) ;
#7907 = FACE_OUTER_BOUND ( 'NONE', #11578, .T. ) ;
#7908 = ORIENTED_EDGE ( 'NONE', *, *, #23732, .T. ) ;
#7909 = DIRECTION ( 'NONE',  ( 0.000000000000000000, 1.000000000000000000, -0.000000000000000000 ) ) ;
#7910 = CIRCLE ( 'NONE', #23517, 8.000000000000000000 ) ;
#7911 = CARTESIAN_POINT ( 'NONE',  ( 5.626939011991851203, -6.906580693685427264, -12.50000000000000000 ) ) ;
#7912 = CARTESIAN_POINT ( 'NONE',  ( -30.00000000000000355, -3.851859888774471706E-31, 9.500000000000000000 ) ) ;
#7913 = EDGE_CURVE ( 'NONE', #5746, #3826, #7481, .T. ) ;
#7914 = FACE_BOUND ( 'NONE', #22660, .T. ) ;
#7915 = ORIENTED_EDGE ( 'NONE', *, *, #3735, .T. ) ;
#7916 = EDGE_CURVE ( 'NONE', #19252, #5444, #23885, .T. ) ;
#7917 = ADVANCED_FACE ( 'NONE', ( #613 ), #19686, .F. ) ;
#7918 = EDGE_LOOP ( 'NONE', ( #5709, #5438, #7688, #111 ) ) ;
#7919 = DIRECTION ( 'NONE',  ( 0.000000000000000000, 0.000000000000000000, 1.000000000000000000 ) ) ;
#7920 = CIRCLE ( 'NONE', #21600, 11.00000000000000355 ) ;
#7921 = CARTESIAN_POINT ( 'NONE',  ( -9.097401919247191771, 2.531095547992308514, 12.07092629224149327 ) ) ;
#7922 = FACE_OUTER_BOUND ( 'NONE', #13847, .T. ) ;
#7923 = CIRCLE ( 'NONE', #23533, 9.500000000000000000 ) ;
#7924 = DIRECTION ( 'NONE',  ( 1.000000000000000000, -0.000000000000000000, 0.000000000000000000 ) ) ;
#7925 = DIRECTION ( 'NONE',  ( 0.000000000000000000, 0.000000000000000000, -1.000000000000000000 ) ) ;
#7926 = AXIS2_PLACEMENT_3D ( 'NONE', #3855, #23759, #12994 ) ;
#7927 = CARTESIAN_POINT ( 'NONE',  ( 5.871322893123448239, 8.081182679344781405, -7.506742014460233037 ) ) ;
#7928 = LINE ( 'NONE', #15377, #3640 ) ;
#7929 = CARTESIAN_POINT ( 'NONE',  ( -5.871322893123450015, -8.081182679344781405, -8.506742014460233037 ) ) ;
#7930 = VECTOR ( 'NONE', #21820, 1000.000000000000000 ) ;
#7931 = VERTEX_POINT ( 'NONE', #1296 ) ;
#7932 = CARTESIAN_POINT ( 'NONE',  ( -29.00000000000000000, 29.49999999999999645, 12.00000000000000000 ) ) ;
#7933 = CARTESIAN_POINT ( 'NONE',  ( -8.680847955711200825, 2.820578480813073607, 7.533165578109189298 ) ) ;
#7934 = FACE_OUTER_BOUND ( 'NONE', #16037, .T. ) ;
#7935 = CARTESIAN_POINT ( 'NONE',  ( 23.85000000000000497, 15.03999999999999915, 27.00000000000000000 ) ) ;
#7936 = VECTOR ( 'NONE', #4662, 1000.000000000000000 ) ;
#7937 = ADVANCED_FACE ( 'NONE', ( #12489 ), #12260, .F. ) ;
#7938 = CIRCLE ( 'NONE', #11435, 1.500000000000000000 ) ;
#7939 = EDGE_LOOP ( 'NONE', ( #14646, #1255, #13610, #22483, #8676, #7534 ) ) ;
#7940 = EDGE_LOOP ( 'NONE', ( #22637, #13195, #15809, #1244, #5471 ) ) ;
#7941 = DIRECTION ( 'NONE',  ( -0.000000000000000000, -0.000000000000000000, -1.000000000000000000 ) ) ;
#7942 = EDGE_CURVE ( 'NONE', #19904, #23803, #17771, .T. ) ;
#7943 = DIRECTION ( 'NONE',  ( 0.000000000000000000, 0.000000000000000000, 1.000000000000000000 ) ) ;
#7944 = ORIENTED_EDGE ( 'NONE', *, *, #14252, .F. ) ;
#7945 = AXIS2_PLACEMENT_3D ( 'NONE', #17918, #4633, #12034 ) ;
#7946 = ORIENTED_EDGE ( 'NONE', *, *, #7702, .F. ) ;
#7947 = DIRECTION ( 'NONE',  ( -0.000000000000000000, -0.000000000000000000, -1.000000000000000000 ) ) ;
#7948 = ADVANCED_FACE ( 'NONE', ( #7010 ), #19951, .T. ) ;
#7949 = ADVANCED_FACE ( 'NONE', ( #12615, #16170 ), #1179, .F. ) ;
#7950 = DIRECTION ( 'NONE',  ( 1.000000000000000000, 0.000000000000000000, 0.000000000000000000 ) ) ;
#7951 = ORIENTED_EDGE ( 'NONE', *, *, #22563, .F. ) ;
#7952 = CARTESIAN_POINT ( 'NONE',  ( -6.963597943683918601, -6.484993096924836387, -3.499616577185218791 ) ) ;
#7953 = EDGE_LOOP ( 'NONE', ( #18910, #1496, #1375, #9414 ) ) ;
#7954 = DIRECTION ( 'NONE',  ( 0.000000000000000000, -1.000000000000000000, 0.000000000000000000 ) ) ;
#7955 = DIRECTION ( 'NONE',  ( -1.000000000000000000, 0.000000000000000000, 0.000000000000000000 ) ) ;
#7956 = DIRECTION ( 'NONE',  ( 0.000000000000000000, 1.000000000000000000, 0.000000000000000000 ) ) ;
#7957 =( BOUNDED_CURVE ( )  B_SPLINE_CURVE ( 2, ( #22630, #6040, #11626, #1017, #17252, #21502, #553, #8309, #15763, #6509, #4803 ),
 .UNSPECIFIED., .F., .F. ) 
 B_SPLINE_CURVE_WITH_KNOTS ( ( 3, 2, 2, 2, 2, 3 ),
 ( 0.6000000000000000888, 0.6200000000000001066, 0.6400000000000001243, 0.6600000000000001421, 0.6800000000000001599, 0.7000000000000000666 ),
 .UNSPECIFIED. ) 
 CURVE ( )  GEOMETRIC_REPRESENTATION_ITEM ( )  RATIONAL_B_SPLINE_CURVE ( ( 0.9999999999999997780, 0.9510565162951537532, 1.000000000000000000, 0.9510565162951535312, 1.000000000000000000, 0.9510565162951535312, 1.000000000000000000, 0.9510565162951535312, 1.000000000000000000, 0.9510565162951533091, 1.000000000000000222 ) ) 
 REPRESENTATION_ITEM ( '' )  );
#7958 = AXIS2_PLACEMENT_3D ( 'NONE', #19526, #176, #10232 ) ;
#7959 = PRODUCT_DEFINITION_CONTEXT ( 'detailed design', #15693, 'design' ) ;
#7960 = VECTOR ( 'NONE', #13701, 1000.000000000000000 ) ;
#7961 = DIRECTION ( 'NONE',  ( -0.000000000000000000, -0.000000000000000000, -1.000000000000000000 ) ) ;
#7962 = VERTEX_POINT ( 'NONE', #23634 ) ;
#7963 = DIRECTION ( 'NONE',  ( -1.000000000000000000, -1.224606353822377258E-16, -0.000000000000000000 ) ) ;
#7964 = FACE_OUTER_BOUND ( 'NONE', #1745, .T. ) ;
#7965 = VERTEX_POINT ( 'NONE', #10311 ) ;
#7966 = AXIS2_PLACEMENT_3D ( 'NONE', #17405, #12267, #21436 ) ;
#7967 = ORIENTED_EDGE ( 'NONE', *, *, #12904, .F. ) ;
#7968 = CARTESIAN_POINT ( 'NONE',  ( -8.680847955710813579, -2.820578480814258437, 3.733165578109188587 ) ) ;
#7969 = ORIENTED_EDGE ( 'NONE', *, *, #17360, .F. ) ;
#7970 = AXIS2_PLACEMENT_3D ( 'NONE', #19553, #9783, #4216 ) ;
#7971 = ORIENTED_EDGE ( 'NONE', *, *, #21097, .F. ) ;
#7972 = EDGE_CURVE ( 'NONE', #5444, #19252, #16096, .T. ) ;
#7973 = VECTOR ( 'NONE', #8378, 1000.000000000000000 ) ;
#7974 = CIRCLE ( 'NONE', #21643, 1.500000000000001998 ) ;
#7975 = ADVANCED_FACE ( 'NONE', ( #14326 ), #1534, .T. ) ;
#7976 = EDGE_LOOP ( 'NONE', ( #17831, #5180, #21034, #4217 ) ) ;
#7977 = EDGE_LOOP ( 'NONE', ( #4753, #8032 ) ) ;
#7978 = PLANE ( 'NONE',  #19995 ) ;
#7979 = CARTESIAN_POINT ( 'NONE',  ( -5.365059087798939252, -7.384370330707086261, -5.933165578109187877 ) ) ;
#7980 = FACE_BOUND ( 'NONE', #13855, .T. ) ;
#7981 = ORIENTED_EDGE ( 'NONE', *, *, #22449, .F. ) ;
#7982 = DIRECTION ( 'NONE',  ( -0.000000000000000000, -0.000000000000000000, -1.000000000000000000 ) ) ;
#7983 = CYLINDRICAL_SURFACE ( 'NONE', #11125, 9.725923461386811297 ) ;
#7984 = EDGE_CURVE ( 'NONE', #5746, #3619, #6116, .T. ) ;
#7985 = ADVANCED_FACE ( 'NONE', ( #9741 ), #20889, .F. ) ;
#7986 = CARTESIAN_POINT ( 'NONE',  ( -33.24999999999999289, -29.50000000000000000, 12.50000000000000000 ) ) ;
#7987 = AXIS2_PLACEMENT_3D ( 'NONE', #15028, #5525, #23967 ) ;
#7988 = VERTEX_POINT ( 'NONE', #20752 ) ;
#7989 = CARTESIAN_POINT ( 'NONE',  ( -31.74999999999995737, 0.000000000000000000, 0.000000000000000000 ) ) ;
#7990 = DIRECTION ( 'NONE',  ( 0.000000000000000000, 0.000000000000000000, 1.000000000000000000 ) ) ;
#7991 = AXIS2_PLACEMENT_3D ( 'NONE', #6219, #621, #23193 ) ;
#7992 = ORIENTED_EDGE ( 'NONE', *, *, #8444, .T. ) ;
#7993 = DIRECTION ( 'NONE',  ( -1.000000000000000000, 0.000000000000000000, 0.000000000000000000 ) ) ;
#7994 = DIRECTION ( 'NONE',  ( -0.000000000000000000, -0.000000000000000000, -1.000000000000000000 ) ) ;
#7995 = CARTESIAN_POINT ( 'NONE',  ( -10.00000000000000000, 0.000000000000000000, 0.000000000000000000 ) ) ;
#7996 = AXIS2_PLACEMENT_3D ( 'NONE', #24040, #12803, #20152 ) ;
#7997 = CARTESIAN_POINT ( 'NONE',  ( 2.935661446562616295, -9.035036904803758873, -5.659589141758144315 ) ) ;
#7998 = CARTESIAN_POINT ( 'NONE',  ( -7.022953521754877748, -5.102474405760673015, -7.833165578109188232 ) ) ;
#7999 = ORIENTED_EDGE ( 'NONE', *, *, #4467, .F. ) ;
#8000 = FILL_AREA_STYLE_COLOUR ( '', #2377 ) ;
#8001 = VERTEX_POINT ( 'NONE', #11321 ) ;
#8002 = ORIENTED_EDGE ( 'NONE', *, *, #12106, .F. ) ;
#8003 = AXIS2_PLACEMENT_3D ( 'NONE', #10620, #5145, #10504 ) ;
#8004 = VERTEX_POINT ( 'NONE', #18799 ) ;
#8005 = AXIS2_PLACEMENT_3D ( 'NONE', #5978, #22344, #13412 ) ;
#8006 = CARTESIAN_POINT ( 'NONE',  ( 11.50000000000000000, -14.80154252341802490, 10.02147513732818851 ) ) ;
#8007 = ORIENTED_EDGE ( 'NONE', *, *, #14039, .T. ) ;
#8008 = CARTESIAN_POINT ( 'NONE',  ( 7.685661446561619314, 5.583959896779020049, -10.25958914175814485 ) ) ;
#8009 = AXIS2_PLACEMENT_3D ( 'NONE', #8635, #6708, #17939 ) ;
#8010 = VECTOR ( 'NONE', #18111, 1000.000000000000000 ) ;
#8011 = PLANE ( 'NONE',  #8710 ) ;
#8012 = LINE ( 'NONE', #9828, #9548 ) ;
#8013 = EDGE_CURVE ( 'NONE', #15214, #7598, #22715, .T. ) ;
#8014 = ORIENTED_EDGE ( 'NONE', *, *, #2464, .T. ) ;
#8015 = CARTESIAN_POINT ( 'NONE',  ( 23.00000000000000000, -13.66196005206961850, -3.918670437617226110 ) ) ;
#8016 = EDGE_CURVE ( 'NONE', #1898, #14307, #16843, .T. ) ;
#8017 = FACE_OUTER_BOUND ( 'NONE', #10808, .T. ) ;
#8018 = DIRECTION ( 'NONE',  ( -1.000000000000000000, 0.000000000000000000, 0.000000000000000000 ) ) ;
#8019 = AXIS2_PLACEMENT_3D ( 'NONE', #5205, #16302, #10559 ) ;
#8020 = DIRECTION ( 'NONE',  ( 0.000000000000000000, -1.000000000000000000, 0.000000000000000000 ) ) ;
#8021 = CARTESIAN_POINT ( 'NONE',  ( -28.99999999999999645, 29.50000000000000000, -3.000000000000000000 ) ) ;
#8022 = DIRECTION ( 'NONE',  ( -0.7052211081716905916, -0.7089874389501501506, -0.000000000000000000 ) ) ;
#8023 = AXIS2_PLACEMENT_3D ( 'NONE', #21067, #11545, #4364 ) ;
#8024 = CARTESIAN_POINT ( 'NONE',  ( 62.94340820527399671, -5.000000000000000000, 6.123233995736775157E-16 ) ) ;
#8025 = ORIENTED_EDGE ( 'NONE', *, *, #22891, .F. ) ;
#8026 = AXIS2_PLACEMENT_3D ( 'NONE', #22223, #23583, #5492 ) ;
#8027 = AXIS2_PLACEMENT_3D ( 'NONE', #10363, #20012, #3293 ) ;
#8028 = ORIENTED_EDGE ( 'NONE', *, *, #268, .T. ) ;
#8029 = DIRECTION ( 'NONE',  ( 0.000000000000000000, 0.2817325568414237313, 0.9594929736144991450 ) ) ;
#8030 = CARTESIAN_POINT ( 'NONE',  ( 2.000000000000000000, 2.449293598294706414E-16, 5.499999999999997335 ) ) ;
#8031 = EDGE_CURVE ( 'NONE', #11436, #16760, #7127, .T. ) ;
#8032 = ORIENTED_EDGE ( 'NONE', *, *, #8564, .F. ) ;
#8033 = DIRECTION ( 'NONE',  ( 0.5735764363510427177, -0.8191520442889941300, 1.003171929053527705E-16 ) ) ;
#8034 = DIRECTION ( 'NONE',  ( 1.000000000000000000, 0.000000000000000000, 0.000000000000000000 ) ) ;
#8035 = EDGE_CURVE ( 'NONE', #5111, #10256, #10231, .T. ) ;
#8036 = CARTESIAN_POINT ( 'NONE',  ( -31.74999999999995737, 0.000000000000000000, 5.000000000000000888 ) ) ;
#8037 = AXIS2_PLACEMENT_3D ( 'NONE', #21012, #4304, #6505 ) ;
#8038 = EDGE_CURVE ( 'NONE', #8836, #2171, #19989, .T. ) ;
#8039 = CARTESIAN_POINT ( 'NONE',  ( 6.507347684473966609, -5.969953219653604037, -12.49999999999999467 ) ) ;
#8040 = EDGE_CURVE ( 'NONE', #21416, #2943, #17680, .T. ) ;
#8041 = CARTESIAN_POINT ( 'NONE',  ( 5.078177448618336420, 0.000000000000000000, 0.000000000000000000 ) ) ;
#8042 = DIRECTION ( 'NONE',  ( 0.000000000000000000, -1.000000000000000000, 0.000000000000000000 ) ) ;
#8043 = ORIENTED_EDGE ( 'NONE', *, *, #6106, .T. ) ;
#8044 = PLANE ( 'NONE',  #21515 ) ;
#8045 = ORIENTED_EDGE ( 'NONE', *, *, #3380, .F. ) ;
#8046 = CARTESIAN_POINT ( 'NONE',  ( 3.230323549912128112, -8.426447456003312908, 12.48391671383376078 ) ) ;
#8047 = CARTESIAN_POINT ( 'NONE',  ( -40.23082370883258108, -27.62204025492846071, -3.000000000000000000 ) ) ;
#8048 = DIRECTION ( 'NONE',  ( 0.000000000000000000, 1.000000000000000000, 0.000000000000000000 ) ) ;
#8049 = DIRECTION ( 'NONE',  ( -1.000000000000000000, 0.000000000000000000, 0.000000000000000000 ) ) ;
#8050 = CARTESIAN_POINT ( 'NONE',  ( 23.00000000000000000, 0.000000000000000000, 0.000000000000000000 ) ) ;
#8051 = LINE ( 'NONE', #17338, #17356 ) ;
#8052 = ORIENTED_EDGE ( 'NONE', *, *, #14977, .F. ) ;
#8053 = CARTESIAN_POINT ( 'NONE',  ( -2.935661446562617183, 9.035036904803758873, -5.806742014460233747 ) ) ;
#8054 = EDGE_LOOP ( 'NONE', ( #17281, #2393, #22362, #22151, #13115, #17456 ) ) ;
#8055 = DIRECTION ( 'NONE',  ( -0.000000000000000000, 0.000000000000000000, 1.000000000000000000 ) ) ;
#8056 = CARTESIAN_POINT ( 'NONE',  ( 8.680847955710813579, 2.820578480814259326, 6.733165578109188587 ) ) ;
#8057 = CARTESIAN_POINT ( 'NONE',  ( 0.000000000000000000, 45.00000000000000000, -8.673617379884035472E-16 ) ) ;
#8058 = EDGE_CURVE ( 'NONE', #4885, #19209, #2844, .T. ) ;
#8059 = CARTESIAN_POINT ( 'NONE',  ( 6.699999999999996625, 0.000000000000000000, 0.000000000000000000 ) ) ;
#8060 = DIRECTION ( 'NONE',  ( -1.000000000000000000, -1.224606353822377258E-16, -0.000000000000000000 ) ) ;
#8061 = EDGE_CURVE ( 'NONE', #22670, #6271, #22063, .T. ) ;
#8062 = VERTEX_POINT ( 'NONE', #7560 ) ;
#8063 = VERTEX_POINT ( 'NONE', #15007 ) ;
#8064 = CONTEXT_DEPENDENT_SHAPE_REPRESENTATION ( #17579, #13146 ) ;
#8065 = ORIENTED_EDGE ( 'NONE', *, *, #6436, .T. ) ;
#8066 = DIRECTION ( 'NONE',  ( 0.000000000000000000, 0.9898214418809322401, 0.1423148382732887240 ) ) ;
#8067 = CARTESIAN_POINT ( 'NONE',  ( 6.809999908187194197E-13, -9.988891130263535700, -8.706742014460230550 ) ) ;
#8068 = VERTEX_POINT ( 'NONE', #22485 ) ;
#8069 = ORIENTED_EDGE ( 'NONE', *, *, #1473, .T. ) ;
#8070 = DIRECTION ( 'NONE',  ( -1.000000000000000000, 0.000000000000000000, 0.000000000000000000 ) ) ;
#8071 = DIRECTION ( 'NONE',  ( -0.7052211081716905916, 0.7089874389501501506, 0.000000000000000000 ) ) ;
#8072 = ORIENTED_EDGE ( 'NONE', *, *, #15623, .T. ) ;
#8073 = CARTESIAN_POINT ( 'NONE',  ( 0.000000000000000000, 0.000000000000000000, 27.00000000000000000 ) ) ;
#8074 = CARTESIAN_POINT ( 'NONE',  ( -40.23082370883260239, 29.50000000000000711, -1.500000000000000000 ) ) ;
#8075 = DIRECTION ( 'NONE',  ( 0.000000000000000000, -1.000000000000000000, 0.000000000000000000 ) ) ;
#8076 = EDGE_CURVE ( 'NONE', #588, #16629, #1304, .T. ) ;
#8077 = CARTESIAN_POINT ( 'NONE',  ( 3.530011532367169913, 0.000000000000000000, 0.000000000000000000 ) ) ;
#8078 = EDGE_LOOP ( 'NONE', ( #15705, #9292, #17316, #12016, #5823 ) ) ;
#8079 = CARTESIAN_POINT ( 'NONE',  ( -10.49999999999999822, 1.285879139104720633E-15, 3.499999999999999556 ) ) ;
#8080 = CARTESIAN_POINT ( 'NONE',  ( 0.000000000000000000, 0.000000000000000000, 27.00000000000000000 ) ) ;
#8081 = DIRECTION ( 'NONE',  ( -1.000000000000000000, -0.000000000000000000, 0.000000000000000000 ) ) ;
#8082 = ORIENTED_EDGE ( 'NONE', *, *, #5021, .F. ) ;
#8083 = CIRCLE ( 'NONE', #14330, 4.999999999999997335 ) ;
#8084 = VERTEX_POINT ( 'NONE', #23447 ) ;
#8085 = CARTESIAN_POINT ( 'NONE',  ( -9.500000000000211386, 3.086737114211961064, 6.959589141758143249 ) ) ;
#8086 = ORIENTED_EDGE ( 'NONE', *, *, #4575, .F. ) ;
#8087 = VERTEX_POINT ( 'NONE', #19672 ) ;
#8088 = EDGE_CURVE ( 'NONE', #14068, #20548, #20758, .T. ) ;
#8089 = VERTEX_POINT ( 'NONE', #14043 ) ;
#8090 = EDGE_CURVE ( 'NONE', #21740, #5942, #4419, .T. ) ;
#8091 = ORIENTED_EDGE ( 'NONE', *, *, #15637, .F. ) ;
#8092 = ORIENTED_EDGE ( 'NONE', *, *, #10368, .F. ) ;
#8093 = CARTESIAN_POINT ( 'NONE',  ( -7.022953521754877748, -5.102474405760673015, -3.833165578109188676 ) ) ;
#8094 = CONICAL_SURFACE ( 'NONE', #11201, 2.024999999999999911, 0.7853981633974743692 ) ;
#8095 = LINE ( 'NONE', #4840, #20805 ) ;
#8096 = EDGE_LOOP ( 'NONE', ( #3690, #20898, #4514, #23620 ) ) ;
#8097 = DIRECTION ( 'NONE',  ( -1.000000000000000000, -1.224606353822377258E-16, -0.000000000000000000 ) ) ;
#8098 = CARTESIAN_POINT ( 'NONE',  ( 67.30704456891035647, 7.562528597612068045E-15, 0.000000000000000000 ) ) ;
#8099 = DIRECTION ( 'NONE',  ( 1.000000000000000000, 0.000000000000000000, 0.000000000000000000 ) ) ;
#8100 = CARTESIAN_POINT ( 'NONE',  ( 0.000000000000000000, 0.000000000000000000, 4.000000000000000000 ) ) ;
#8101 = VECTOR ( 'NONE', #18601, 1000.000000000000000 ) ;
#8102 = ORIENTED_EDGE ( 'NONE', *, *, #9494, .T. ) ;
#8103 = COLOUR_RGB ( '',0.7921568627450980005, 0.8196078431372548767, 0.9333333333333333481 ) ;
#8104 = CARTESIAN_POINT ( 'NONE',  ( 23.00000000000000000, 0.000000000000000000, 0.000000000000000000 ) ) ;
#8105 = ORIENTED_EDGE ( 'NONE', *, *, #10676, .T. ) ;
#8106 = CARTESIAN_POINT ( 'NONE',  ( 0.000000000000000000, -14.99147757894464306, 7.750000000000000000 ) ) ;
#8107 = CARTESIAN_POINT ( 'NONE',  ( -1.999999999999994449, -45.00000000000000000, -23.99999999999999645 ) ) ;
#8108 = EDGE_CURVE ( 'NONE', #1766, #3022, #8538, .T. ) ;
#8109 = FACE_BOUND ( 'NONE', #7348, .T. ) ;
#8110 = CARTESIAN_POINT ( 'NONE',  ( -5.365059087798940141, -7.384370330707086261, -5.933165578109187877 ) ) ;
#8111 = CLOSED_SHELL ( 'NONE', ( #13261, #365, #23525, #3642, #503, #17102, #11269, #6254 ) ) ;
#8112 = ORIENTED_EDGE ( 'NONE', *, *, #17664, .F. ) ;
#8113 = EDGE_CURVE ( 'NONE', #1818, #23864, #14140, .T. ) ;
#8114 = DIRECTION ( 'NONE',  ( -1.000000000000000000, -0.000000000000000000, -0.000000000000000000 ) ) ;
#8115 = ORIENTED_EDGE ( 'NONE', *, *, #7703, .F. ) ;
#8116 = EDGE_LOOP ( 'NONE', ( #16429, #18795, #3181, #19268 ) ) ;
#8117 = CARTESIAN_POINT ( 'NONE',  ( 5.365059087799946447, -7.384370330706356178, 8.333165578109190008 ) ) ;
#8118 = EDGE_CURVE ( 'NONE', #21512, #14945, #12959, .T. ) ;
#8119 = EDGE_CURVE ( 'NONE', #20703, #9099, #496, .T. ) ;
#8120 = ADVANCED_FACE ( 'NONE', ( #15743 ), #4781, .F. ) ;
#8121 = ORIENTED_EDGE ( 'NONE', *, *, #15877, .F. ) ;
#8122 = VECTOR ( 'NONE', #2698, 1000.000000000000000 ) ;
#8123 = FACE_OUTER_BOUND ( 'NONE', #3167, .T. ) ;
#8124 = VERTEX_POINT ( 'NONE', #12325 ) ;
#8125 = CARTESIAN_POINT ( 'NONE',  ( -1.000000000000000222, 0.000000000000000000, 4.000000000000000000 ) ) ;
#8126 = UNCERTAINTY_MEASURE_WITH_UNIT (LENGTH_MEASURE( 1.000000000000000082E-05 ), #13162, 'distance_accuracy_value', 'NONE');
#8127 = CARTESIAN_POINT ( 'NONE',  ( -10.00000000000000000, 0.000000000000000000, 0.000000000000000000 ) ) ;
#8128 = CARTESIAN_POINT ( 'NONE',  ( -9.500000000000000000, -6.482511860946779655E-13, 4.206742014460233214 ) ) ;
#8129 = CYLINDRICAL_SURFACE ( 'NONE', #11082, 1.500000000000001332 ) ;
#8130 = ADVANCED_BREP_SHAPE_REPRESENTATION ( '', ( #18892, #8005 ), #1445 ) ;
#8131 = DIRECTION ( 'NONE',  ( 1.000000000000000000, -2.600433232233976523E-16, 0.000000000000000000 ) ) ;
#8132 = CARTESIAN_POINT ( 'NONE',  ( -42.00000000000001421, -26.82133436441677432, 11.58578643762690596 ) ) ;
#8133 = CARTESIAN_POINT ( 'NONE',  ( 20.99999999999999645, -29.50000000000000355, 11.50000000000000000 ) ) ;
#8134 = CYLINDRICAL_SURFACE ( 'NONE', #2825, 1.999999999999994449 ) ;
#8135 = FACE_OUTER_BOUND ( 'NONE', #3560, .T. ) ;
#8136 = ADVANCED_FACE ( 'NONE', ( #17835 ), #6488, .F. ) ;
#8137 = CARTESIAN_POINT ( 'NONE',  ( 77.78386452199872281, 7.420530141404717394E-15, 0.000000000000000000 ) ) ;
#8138 = VERTEX_POINT ( 'NONE', #19795 ) ;
#8139 = CARTESIAN_POINT ( 'NONE',  ( -9.499999999999790390, -3.086737114213257804, -12.30674201446023197 ) ) ;
#8140 = ORIENTED_EDGE ( 'NONE', *, *, #42, .T. ) ;
#8141 = VERTEX_POINT ( 'NONE', #4661 ) ;
#8142 = DIRECTION ( 'NONE',  ( 1.000000000000000000, 2.600433232233976523E-16, 0.000000000000000000 ) ) ;
#8143 = CARTESIAN_POINT ( 'NONE',  ( 7.000000000000000888, 0.000000000000000000, 14.72592346043842326 ) ) ;
#8144 = EDGE_CURVE ( 'NONE', #6052, #18241, #17563, .T. ) ;
#8145 = ORIENTED_EDGE ( 'NONE', *, *, #4198, .T. ) ;
#8146 = CARTESIAN_POINT ( 'NONE',  ( 665.5295305079686159, 872.2216676388150063, 1283.253407838750491 ) ) ;
#8147 = CARTESIAN_POINT ( 'NONE',  ( 30.16774287754691386, -40.66994976491903913, -3.000000000000000000 ) ) ;
#8148 = AXIS2_PLACEMENT_3D ( 'NONE', #6910, #23635, #10431 ) ;
#8149 = CARTESIAN_POINT ( 'NONE',  ( -31.74999999999995737, 6.123233995736767268E-16, -5.000000000000000888 ) ) ;
#8150 = CARTESIAN_POINT ( 'NONE',  ( 70.51113724927145654, 6.123233995736675563E-16, -5.000000000000007994 ) ) ;
#8151 = CARTESIAN_POINT ( 'NONE',  ( -40.23082370883260239, 29.50000000000000711, -3.000000000000000000 ) ) ;
#8152 = LINE ( 'NONE', #15596, #14207 ) ;
#8153 = DIRECTION ( 'NONE',  ( -0.000000000000000000, -0.000000000000000000, -1.000000000000000000 ) ) ;
#8154 = CARTESIAN_POINT ( 'NONE',  ( 75.45454545454545325, 7.491529369508391930E-15, 0.000000000000000000 ) ) ;
#8155 = ORIENTED_EDGE ( 'NONE', *, *, #2601, .T. ) ;
#8156 = DIRECTION ( 'NONE',  ( -0.000000000000000000, -0.000000000000000000, -1.000000000000000000 ) ) ;
#8157 = ORIENTED_EDGE ( 'NONE', *, *, #14691, .F. ) ;
#8158 = DIRECTION ( 'NONE',  ( 1.000000000000000000, 0.000000000000000000, 0.000000000000000000 ) ) ;
#8159 = CYLINDRICAL_SURFACE ( 'NONE', #148, 1.500000000000000000 ) ;
#8160 = CARTESIAN_POINT ( 'NONE',  ( 0.000000000000000000, -13.66196005206961850, -3.918670437617226110 ) ) ;
#8161 = AXIS2_PLACEMENT_3D ( 'NONE', #14045, #5029, #23338 ) ;
#8162 = CARTESIAN_POINT ( 'NONE',  ( 41.00000000000000000, 0.000000000000000000, 11.00000000000000000 ) ) ;
#8163 = EDGE_CURVE ( 'NONE', #23091, #23565, #10991, .T. ) ;
#8164 = ORIENTED_EDGE ( 'NONE', *, *, #7526, .T. ) ;
#8165 = CARTESIAN_POINT ( 'NONE',  ( 40.00000000000000000, -29.50000000000000000, -27.00000000000000000 ) ) ;
#8166 = CARTESIAN_POINT ( 'NONE',  ( 1.999999999999994449, -45.00000000000000000, 26.97499999999999432 ) ) ;
#8167 = ORIENTED_EDGE ( 'NONE', *, *, #24056, .F. ) ;
#8168 = CARTESIAN_POINT ( 'NONE',  ( 9.500000000000209610, -3.086737114211962396, -5.106742014460234458 ) ) ;
#8169 = VERTEX_POINT ( 'NONE', #6355 ) ;
#8170 = EDGE_CURVE ( 'NONE', #23971, #17518, #10110, .T. ) ;
#8171 = CARTESIAN_POINT ( 'NONE',  ( 8.680847955711199049, -2.820578480813074496, 8.533165578109187521 ) ) ;
#8172 = EDGE_CURVE ( 'NONE', #15320, #6823, #22958, .T. ) ;
#8173 = CARTESIAN_POINT ( 'NONE',  ( -31.74999999999995737, 0.000000000000000000, 5.000000000000000888 ) ) ;
#8174 = DIRECTION ( 'NONE',  ( -1.000000000000000000, -1.224606353822377258E-16, -0.000000000000000000 ) ) ;
#8175 = ORIENTED_EDGE ( 'NONE', *, *, #13668, .T. ) ;
#8177 = ORIENTED_EDGE ( 'NONE', *, *, #16616, .T. ) ;
#8176 = PRESENTATION_LAYER_ASSIGNMENT (  '', '', ( #14055 ) ) ;
#8178 = ITEM_DEFINED_TRANSFORMATION ( 'NONE', 'NONE', #18949,  #8005 ) ;
#8179 = EDGE_LOOP ( 'NONE', ( #1378, #10106 ) ) ;
#8180 = CARTESIAN_POINT ( 'NONE',  ( 15.00000000000000355, 15.50000000000000000, 7.700000000000001954 ) ) ;
#8181 = CARTESIAN_POINT ( 'NONE',  ( 9.500000000000000000, 6.470877716354879437E-13, -13.20674201446023410 ) ) ;
#8182 = ORIENTED_EDGE ( 'NONE', *, *, #4791, .T. ) ;
#8183 = ADVANCED_FACE ( 'NONE', ( #23206 ), #16090, .F. ) ;
#8184 = FACE_BOUND ( 'NONE', #23595, .T. ) ;
#8185 = ORIENTED_EDGE ( 'NONE', *, *, #1, .F. ) ;
#8186 = CARTESIAN_POINT ( 'NONE',  ( -2.018988670968663524, -9.287031262157933398, -3.500000381810258077 ) ) ;
#8187 = EDGE_CURVE ( 'NONE', #13405, #17583, #3975, .T. ) ;
#8188 = ORIENTED_EDGE ( 'NONE', *, *, #10738, .T. ) ;
#8189 = DIRECTION ( 'NONE',  ( 0.000000000000000000, -1.000000000000000000, 0.000000000000000000 ) ) ;
#8190 = DIRECTION ( 'NONE',  ( -0.5735764363510519326, 0.8191520442889876907, 1.003171929053519816E-16 ) ) ;
#8191 = CARTESIAN_POINT ( 'NONE',  ( 85.63636363636365445, 7.491529369508391930E-15, 0.000000000000000000 ) ) ;
#8192 = ADVANCED_FACE ( 'NONE', ( #15875 ), #3618, .T. ) ;
#8193 = CARTESIAN_POINT ( 'NONE',  ( 9.500000000000000000, 6.470877716354879437E-13, 7.206742014460234103 ) ) ;
#8194 = ORIENTED_EDGE ( 'NONE', *, *, #11240, .T. ) ;
#8195 = APPLICATION_CONTEXT ( 'automotive_design' ) ;
#8196 = LINE ( 'NONE', #19453, #1721 ) ;
#8197 = EDGE_CURVE ( 'NONE', #13932, #14909, #21556, .T. ) ;
#8198 = DIRECTION ( 'NONE',  ( 0.000000000000000000, -1.000000000000000000, 0.000000000000000000 ) ) ;
#8199 = CARTESIAN_POINT ( 'NONE',  ( 14.51962751333974211, -3.765689428759034563, 8.721787840009190163 ) ) ;
#8200 = ORIENTED_EDGE ( 'NONE', *, *, #7427, .F. ) ;
#8201 = ORIENTED_EDGE ( 'NONE', *, *, #5661, .T. ) ;
#8202 = CARTESIAN_POINT ( 'NONE',  ( 9.500000000000000000, 6.470877716354879437E-13, 4.059589141758143782 ) ) ;
#8203 = VERTEX_POINT ( 'NONE', #8786 ) ;
#8204 = ORIENTED_EDGE ( 'NONE', *, *, #21227, .T. ) ;
#8205 = ORIENTED_EDGE ( 'NONE', *, *, #16220, .F. ) ;
#8206 = DIRECTION ( 'NONE',  ( 0.000000000000000000, 0.000000000000000000, 1.000000000000000000 ) ) ;
#8207 = CARTESIAN_POINT ( 'NONE',  ( 66.14750088563508257, 7.420530141404717394E-15, 0.000000000000000000 ) ) ;
#8208 = PRODUCT_RELATED_PRODUCT_CATEGORY ( 'part', '', ( #10186 ) ) ;
#8209 = DIRECTION ( 'NONE',  ( 0.000000000000000000, -1.000000000000000000, 0.000000000000000000 ) ) ;
#8210 = AXIS2_PLACEMENT_3D ( 'NONE', #21486, #13795, #17945 ) ;
#8211 = ORIENTED_EDGE ( 'NONE', *, *, #10177, .T. ) ;
#8212 = DIRECTION ( 'NONE',  ( 1.000000000000000000, 0.000000000000000000, 0.000000000000000000 ) ) ;
#8213 = CARTESIAN_POINT ( 'NONE',  ( -34.00000000000000000, -3.851859888774471706E-31, 10.49999999999999822 ) ) ;
#8214 = DIRECTION ( 'NONE',  ( -1.000000000000000000, -0.000000000000000000, -0.000000000000000000 ) ) ;
#8215 = EDGE_CURVE ( 'NONE', #6174, #17524, #2047, .T. ) ;
#8216 = DIRECTION ( 'NONE',  ( -0.000000000000000000, -0.000000000000000000, -1.000000000000000000 ) ) ;
#8217 = AXIS2_PLACEMENT_3D ( 'NONE', #14952, #22187, #3504 ) ;
#8218 = ORIENTED_EDGE ( 'NONE', *, *, #11080, .T. ) ;
#8219 = CARTESIAN_POINT ( 'NONE',  ( 6.809999908187194197E-13, -9.988891130263535700, 7.559589141758143782 ) ) ;
#8220 = EDGE_CURVE ( 'NONE', #2794, #8913, #895, .T. ) ;
#8221 = EDGE_CURVE ( 'NONE', #581, #14771, #20377, .T. ) ;
#8222 = ORIENTED_EDGE ( 'NONE', *, *, #23513, .T. ) ;
#8223 = DIRECTION ( 'NONE',  ( -0.000000000000000000, -0.000000000000000000, 1.000000000000000000 ) ) ;
#8224 = LINE ( 'NONE', #14213, #13699 ) ;
#8225 = CARTESIAN_POINT ( 'NONE',  ( -15.00000000000000178, -0.3238088414458164532, 9.499999999999998224 ) ) ;
#8226 = LINE ( 'NONE', #12013, #20064 ) ;
#8227 = CARTESIAN_POINT ( 'NONE',  ( 6.222797240145152671E-13, -9.127583699786111282, -6.133165578109188054 ) ) ;
#8228 = CARTESIAN_POINT ( 'NONE',  ( 80.39795365981946418, 5.000000000000015099, 0.000000000000000000 ) ) ;
#8229 = VERTEX_POINT ( 'NONE', #12679 ) ;
#8230 = ORIENTED_EDGE ( 'NONE', *, *, #24004, .F. ) ;
#8231 = AXIS2_PLACEMENT_3D ( 'NONE', #15468, #2668, #4379 ) ;
#8232 = CARTESIAN_POINT ( 'NONE',  ( 6.222797240145152671E-13, -9.127583699786111282, 8.133165578109188942 ) ) ;
#8233 = VECTOR ( 'NONE', #20557, 1000.000000000000000 ) ;
#8234 = AXIS2_PLACEMENT_3D ( 'NONE', #2485, #9769, #5897 ) ;
#8235 = ORIENTED_EDGE ( 'NONE', *, *, #10397, .T. ) ;
#8236 = DIRECTION ( 'NONE',  ( 2.212827668532963360E-19, 1.040824735884519909E-17, 1.000000000000000000 ) ) ;
#8237 = ORIENTED_EDGE ( 'NONE', *, *, #21567, .F. ) ;
#8238 = ORIENTED_EDGE ( 'NONE', *, *, #15769, .T. ) ;
#8239 = DIRECTION ( 'NONE',  ( -1.000000000000000000, -1.224606353822377258E-16, -0.000000000000000000 ) ) ;
#8240 = CYLINDRICAL_SURFACE ( 'NONE', #2598, 8.999999999999994671 ) ;
#8241 = PRODUCT_DEFINITION ( 'UNKNOWN', '', #18571, #13589 ) ;
#8242 = EDGE_CURVE ( 'NONE', #15214, #3810, #1710, .T. ) ;
#8243 = DIRECTION ( 'NONE',  ( 0.000000000000000000, 0.000000000000000000, 1.000000000000000000 ) ) ;
#8244 = CARTESIAN_POINT ( 'NONE',  ( 4.029965094393306726E-41, -5.916456789157588541E-28, 12.50000000000000000 ) ) ;
#8245 = ORIENTED_EDGE ( 'NONE', *, *, #1616, .F. ) ;
#8246 = CARTESIAN_POINT ( 'NONE',  ( -2.999999999999996447, 6.000000000000000000, 98.99999999999998579 ) ) ;
#8247 = EDGE_CURVE ( 'NONE', #22492, #6266, #14512, .T. ) ;
#8248 = DIRECTION ( 'NONE',  ( -1.000000000000000000, -0.000000000000000000, -0.000000000000000000 ) ) ;
#8249 = AXIS2_PLACEMENT_3D ( 'NONE', #14243, #24006, #16071 ) ;
#8250 = CONICAL_SURFACE ( 'NONE', #19175, 9.000000000000000000, 0.7853981633974509435 ) ;
#8251 = EDGE_CURVE ( 'NONE', #17534, #22408, #1364, .T. ) ;
#8252 = AXIS2_PLACEMENT_3D ( 'NONE', #3184, #16353, #20382 ) ;
#8253 = CARTESIAN_POINT ( 'NONE',  ( 33.99999999999998579, -1.387778780781445676E-14, 9.500000000000000000 ) ) ;
#8254 = AXIS2_PLACEMENT_3D ( 'NONE', #8021, #7768, #6207 ) ;
#8255 = EDGE_CURVE ( 'NONE', #15773, #2680, #16464, .T. ) ;
#8256 = DIRECTION ( 'NONE',  ( -1.000000000000000000, -1.224606353822377258E-16, -0.000000000000000000 ) ) ;
#8257 = LINE ( 'NONE', #2304, #9404 ) ;
#8258 = AXIS2_PLACEMENT_3D ( 'NONE', #15779, #2847, #10022 ) ;
#8259 = DIRECTION ( 'NONE',  ( 1.000000000000000000, 0.000000000000000000, 0.000000000000000000 ) ) ;
#8260 = AXIS2_PLACEMENT_3D ( 'NONE', #10411, #3920, #10974 ) ;
#8261 = AXIS2_PLACEMENT_3D ( 'NONE', #23804, #12556, #3313 ) ;
#8262 = DIRECTION ( 'NONE',  ( -0.000000000000000000, -0.000000000000000000, -1.000000000000000000 ) ) ;
#8263 = VERTEX_POINT ( 'NONE', #8651 ) ;
#8264 = CARTESIAN_POINT ( 'NONE',  ( 2.935661446562616295, -9.035036904803758873, -12.80674201446023375 ) ) ;
#8265 = VERTEX_POINT ( 'NONE', #14388 ) ;
#8266 = EDGE_LOOP ( 'NONE', ( #9906, #3155 ) ) ;
#8267 = CARTESIAN_POINT ( 'NONE',  ( 9.500000000000209610, -3.086737114211962396, 3.959589141758145026 ) ) ;
#8268 = CARTESIAN_POINT ( 'NONE',  ( 9.500000000000209610, -3.086737114211962396, 13.10674201446023091 ) ) ;
#8269 = ORIENTED_EDGE ( 'NONE', *, *, #12322, .T. ) ;
#8270 =( LENGTH_UNIT ( ) NAMED_UNIT ( * ) SI_UNIT ( .MILLI., .METRE. ) );
#8271 = DIRECTION ( 'NONE',  ( -1.000000000000000000, -0.000000000000000000, -0.000000000000000000 ) ) ;
#8272 = CARTESIAN_POINT ( 'NONE',  ( 0.000000000000000000, -4.685197434473820088, 9.540979117872439019E-15 ) ) ;
#8273 = CIRCLE ( 'NONE', #13737, 8.000000000000000000 ) ;
#8274 = CIRCLE ( 'NONE', #21929, 17.25000000000000000 ) ;
#8275 = CONICAL_SURFACE ( 'NONE', #21930, 4.172000000000008590, 0.9599310885968742602 ) ;
#8276 = CARTESIAN_POINT ( 'NONE',  ( -2.935661446562617183, 9.035036904803758873, 6.659589141758144315 ) ) ;
#8277 = AXIS2_PLACEMENT_3D ( 'NONE', #350, #15091, #20857 ) ;
#8278 = EDGE_CURVE ( 'NONE', #2680, #11511, #11825, .T. ) ;
#8279 = AXIS2_PLACEMENT_3D ( 'NONE', #10846, #18316, #1597 ) ;
#8280 = CARTESIAN_POINT ( 'NONE',  ( 50.00005079999999680, 0.000000000000000000, 0.000000000000000000 ) ) ;
#8281 = CARTESIAN_POINT ( 'NONE',  ( 9.500000000000000000, 6.470877716354879437E-13, -8.059589141758143782 ) ) ;
#8282 = CIRCLE ( 'NONE', #4409, 5.999999999999998224 ) ;
#8283 = LINE ( 'NONE', #21240, #17208 ) ;
#8284 = ORIENTED_EDGE ( 'NONE', *, *, #16262, .F. ) ;
#8285 = DIRECTION ( 'NONE',  ( -1.000000000000000000, -1.224606353822377258E-16, -0.000000000000000000 ) ) ;
#8286 = ADVANCED_FACE ( 'NONE', ( #14500 ), #16453, .F. ) ;
#8287 = EDGE_CURVE ( 'NONE', #8820, #24058, #15280, .T. ) ;
#8288 = ORIENTED_EDGE ( 'NONE', *, *, #606, .F. ) ;
#8289 = CARTESIAN_POINT ( 'NONE',  ( 86.21613547800127719, 7.562528597612068045E-15, 0.000000000000000000 ) ) ;
#8290 = DIRECTION ( 'NONE',  ( 1.000000000000000000, 0.000000000000000000, -0.000000000000000000 ) ) ;
#8291 = DIRECTION ( 'NONE',  ( -1.000000000000000000, 0.000000000000000000, 0.000000000000000000 ) ) ;
#8292 = FACE_OUTER_BOUND ( 'NONE', #13772, .T. ) ;
#8293 = VECTOR ( 'NONE', #17081, 1000.000000000000000 ) ;
#8294 = DIRECTION ( 'NONE',  ( 0.000000000000000000, 0.000000000000000000, 1.000000000000000000 ) ) ;
#8295 = ORIENTED_EDGE ( 'NONE', *, *, #18228, .F. ) ;
#8296 = TOROIDAL_SURFACE ( 'NONE', #15303, 3.500000000000001776, 1.500000000000000000 ) ;
#8297 = LINE ( 'NONE', #15751, #11400 ) ;
#8298 = DIRECTION ( 'NONE',  ( 0.000000000000000000, 0.000000000000000000, -1.000000000000000000 ) ) ;
#8299 = AXIS2_PLACEMENT_3D ( 'NONE', #23642, #21904, #16179 ) ;
#8300 = EDGE_LOOP ( 'NONE', ( #2900, #408, #4389, #5148 ) ) ;
#8301 = CARTESIAN_POINT ( 'NONE',  ( 9.500000000000209610, -3.086737114211962396, -7.106742014460232681 ) ) ;
#8302 = ORIENTED_EDGE ( 'NONE', *, *, #1510, .F. ) ;
#8303 = AXIS2_PLACEMENT_3D ( 'NONE', #10977, #3689, #5647 ) ;
#8304 = CARTESIAN_POINT ( 'NONE',  ( -20.85000000000000142, -15.03999999999999915, -27.00000000000000000 ) ) ;
#8305 = CARTESIAN_POINT ( 'NONE',  ( -5.365059087799948223, 7.384370330706355290, 9.333165578109190008 ) ) ;
#8306 = VECTOR ( 'NONE', #3525, 1000.000000000000000 ) ;
#8307 = CARTESIAN_POINT ( 'NONE',  ( 40.89823313241238623, -26.41789760203348081, -27.00000000000000000 ) ) ;
#8308 = DIRECTION ( 'NONE',  ( 0.4999999999999998890, 0.8660254037844385966, 0.000000000000000000 ) ) ;
#8309 = CARTESIAN_POINT ( 'NONE',  ( -5.871322893123449127, -8.081182679344781405, 5.359589141758143604 ) ) ;
#8310 = EDGE_LOOP ( 'NONE', ( #21477, #9802, #5731, #10382 ) ) ;
#8311 = AXIS2_PLACEMENT_3D ( 'NONE', #23689, #5026, #1235 ) ;
#8312 = ORIENTED_EDGE ( 'NONE', *, *, #7197, .T. ) ;
#8313 = LINE ( 'NONE', #13823, #6847 ) ;
#8314 = AXIS2_PLACEMENT_3D ( 'NONE', #11616, #19083, #9772 ) ;
#8315 = CIRCLE ( 'NONE', #5596, 5.000000000000000888 ) ;
#8316 = CARTESIAN_POINT ( 'NONE',  ( -5.871322893124554021, 8.081182679343978492, -9.906742014460235168 ) ) ;
#8317 = ORIENTED_EDGE ( 'NONE', *, *, #12020, .T. ) ;
#8318 = CIRCLE ( 'NONE', #16116, 6.050000000006052758 ) ;
#8319 = ORIENTED_EDGE ( 'NONE', *, *, #2738, .T. ) ;
#8320 = CARTESIAN_POINT ( 'NONE',  ( -6.503161203208929209, -6.562476031654467690, -12.26909456176216828 ) ) ;
#8321 = AXIS2_PLACEMENT_3D ( 'NONE', #2247, #5903, #18975 ) ;
#8322 = EDGE_CURVE ( 'NONE', #19925, #2741, #19213, .T. ) ;
#8323 = DIRECTION ( 'NONE',  ( -0.000000000000000000, -0.000000000000000000, 1.000000000000000000 ) ) ;
#8324 = VECTOR ( 'NONE', #18377, 1000.000000000000000 ) ;
#8325 = VERTEX_POINT ( 'NONE', #5843 ) ;
#8326 = LINE ( 'NONE', #16257, #12765 ) ;
#8327 = ORIENTED_EDGE ( 'NONE', *, *, #12173, .F. ) ;
#8328 = LINE ( 'NONE', #17735, #4381 ) ;
#8329 = DIRECTION ( 'NONE',  ( -0.000000000000000000, -0.000000000000000000, -1.000000000000000000 ) ) ;
#8330 = DIRECTION ( 'NONE',  ( 0.000000000000000000, 0.000000000000000000, 1.000000000000000000 ) ) ;
#8331 = CARTESIAN_POINT ( 'NONE',  ( -1.000000000000000222, 0.000000000000000000, 0.2999999999999990452 ) ) ;
#8332 = ORIENTED_EDGE ( 'NONE', *, *, #15527, .F. ) ;
#8333 = DIRECTION ( 'NONE',  ( 0.000000000000000000, -1.000000000000000000, 0.000000000000000000 ) ) ;
#8334 = CARTESIAN_POINT ( 'NONE',  ( 29.00000000000000711, -29.50000000000000711, 27.00000000000000000 ) ) ;
#8335 = CARTESIAN_POINT ( 'NONE',  ( -41.73082370883260950, 27.62204025492845716, 0.000000000000000000 ) ) ;
#8336 = ORIENTED_EDGE ( 'NONE', *, *, #14272, .F. ) ;
#8337 = CARTESIAN_POINT ( 'NONE',  ( -6.822232771736903637E-13, 9.988891130263535700, 6.559589141758143782 ) ) ;
#8338 = VECTOR ( 'NONE', #15887, 1000.000000000000000 ) ;
#8339 = ORIENTED_EDGE ( 'NONE', *, *, #5868, .F. ) ;
#8340 = CONICAL_SURFACE ( 'NONE', #16904, 4.172000000000008590, 0.9599310885968742602 ) ;
#8341 = ORIENTED_EDGE ( 'NONE', *, *, #5608, .F. ) ;
#8342 = ADVANCED_FACE ( 'NONE', ( #13267 ), #16703, .T. ) ;
#8343 = CONICAL_SURFACE ( 'NONE', #4070, 2.024999999999999911, 0.7853981633974743692 ) ;
#8344 = AXIS2_PLACEMENT_3D ( 'NONE', #17136, #436, #4224 ) ;
#8345 = VECTOR ( 'NONE', #23886, 1000.000000000000000 ) ;
#8346 = ORIENTED_EDGE ( 'NONE', *, *, #18705, .F. ) ;
#8347 = EDGE_CURVE ( 'NONE', #3463, #16756, #9424, .T. ) ;
#8348 = CARTESIAN_POINT ( 'NONE',  ( 2.682529543899157876, 8.255977015246598327, -5.033165578109189298 ) ) ;
#8349 = CARTESIAN_POINT ( 'NONE',  ( 0.000000000000000000, 0.000000000000000000, 12.00000000000000000 ) ) ;
#8350 = DIRECTION ( 'NONE',  ( 0.000000000000000000, 0.000000000000000000, -1.000000000000000000 ) ) ;
#8351 = ORIENTED_EDGE ( 'NONE', *, *, #14030, .T. ) ;
#8352 = CARTESIAN_POINT ( 'NONE',  ( -15.56475192642547967, -5.220978644676160130, -7.947934502462941531 ) ) ;
#8353 = DIRECTION ( 'NONE',  ( -0.000000000000000000, -0.000000000000000000, 1.000000000000000000 ) ) ;
#8354 = EDGE_CURVE ( 'NONE', #128, #11857, #5968, .T. ) ;
#8355 = DIRECTION ( 'NONE',  ( -1.000000000000000000, 0.000000000000000000, 0.000000000000000000 ) ) ;
#8356 = VERTEX_POINT ( 'NONE', #20863 ) ;
#8357 = DIRECTION ( 'NONE',  ( -0.000000000000000000, -0.000000000000000000, -1.000000000000000000 ) ) ;
#8358 = CARTESIAN_POINT ( 'NONE',  ( 29.00000000000000355, -29.50000000000000000, -3.000000000000000000 ) ) ;
#8359 = CIRCLE ( 'NONE', #11450, 9.999999999999998224 ) ;
#8360 = CIRCLE ( 'NONE', #13426, 1.499999999999999778 ) ;
#8361 = DIRECTION ( 'NONE',  ( 0.000000000000000000, 0.000000000000000000, -1.000000000000000000 ) ) ;
#8362 = AXIS2_PLACEMENT_3D ( 'NONE', #27, #19504, #9375 ) ;
#8363 = DIRECTION ( 'NONE',  ( -1.000000000000000000, -0.000000000000000000, -0.000000000000000000 ) ) ;
#8364 = AXIS2_PLACEMENT_3D ( 'NONE', #9717, #18901, #2052 ) ;
#8365 = DIRECTION ( 'NONE',  ( 0.000000000000000000, -1.000000000000000000, 0.000000000000000000 ) ) ;
#8366 = CARTESIAN_POINT ( 'NONE',  ( -5.365059087799948223, 7.384370330706355290, -9.333165578109190008 ) ) ;
#8367 = ORIENTED_EDGE ( 'NONE', *, *, #23289, .F. ) ;
#8368 = CIRCLE ( 'NONE', #9519, 1.000000000000000222 ) ;
#8369 = FACE_OUTER_BOUND ( 'NONE', #12248, .T. ) ;
#8370 = ORIENTED_EDGE ( 'NONE', *, *, #4965, .T. ) ;
#8371 = ORIENTED_EDGE ( 'NONE', *, *, #20335, .F. ) ;
#8372 = CARTESIAN_POINT ( 'NONE',  ( 2.682529543899157876, 8.255977015246598327, 9.033165578109187521 ) ) ;
#8373 = ORIENTED_EDGE ( 'NONE', *, *, #22832, .T. ) ;
#8374 = DIRECTION ( 'NONE',  ( -3.382732168450096629E-16, -6.865389797465756195E-17, 0.9999999999999998890 ) ) ;
#8375 = DIRECTION ( 'NONE',  ( 0.000000000000000000, -1.000000000000000000, 0.000000000000000000 ) ) ;
#8376 = ORIENTED_EDGE ( 'NONE', *, *, #5661, .F. ) ;
#8377 = EDGE_CURVE ( 'NONE', #16629, #588, #12558, .T. ) ;
#8378 = DIRECTION ( 'NONE',  ( 0.000000000000000000, -0.5000000000000013323, -0.8660254037844379305 ) ) ;
#8379 = DIRECTION ( 'NONE',  ( 0.000000000000000000, -1.000000000000000000, 0.000000000000000000 ) ) ;
#8380 = UNCERTAINTY_MEASURE_WITH_UNIT (LENGTH_MEASURE( 1.000000000000000082E-05 ), #7780, 'distance_accuracy_value', 'NONE');
#8381 = EDGE_CURVE ( 'NONE', #9521, #6981, #4013, .T. ) ;
#8382 = AXIS2_PLACEMENT_3D ( 'NONE', #18598, #16740, #18345 ) ;
#8383 = CARTESIAN_POINT ( 'NONE',  ( -2.601798256281209198, 8.616464066528292776, 100.5062743227686752 ) ) ;
#8384 = CYLINDRICAL_SURFACE ( 'NONE', #11517, 20.85000000000000853 ) ;
#8385 = DIRECTION ( 'NONE',  ( -0.000000000000000000, -0.000000000000000000, -1.000000000000000000 ) ) ;
#8386 = ORIENTED_EDGE ( 'NONE', *, *, #15393, .F. ) ;
#8387 = VECTOR ( 'NONE', #21319, 1000.000000000000000 ) ;
#8388 = ORIENTED_EDGE ( 'NONE', *, *, #16218, .T. ) ;
#8389 = TOROIDAL_SURFACE ( 'NONE', #7224, 14.02592346138681201, 0.2999999999999999334 ) ;
#8390 = DIRECTION ( 'NONE',  ( -1.000000000000000000, -2.600433232233976523E-16, 0.000000000000000000 ) ) ;
#8391 = FACE_OUTER_BOUND ( 'NONE', #7291, .T. ) ;
#8392 = FACE_OUTER_BOUND ( 'NONE', #1398, .T. ) ;
#8393 = ORIENTED_EDGE ( 'NONE', *, *, #2463, .T. ) ;
#8394 = DIRECTION ( 'NONE',  ( -0.000000000000000000, -0.000000000000000000, 1.000000000000000000 ) ) ;
#8395 = CARTESIAN_POINT ( 'NONE',  ( 20.85000000000000497, -16.67999999999999616, 13.50000000000000178 ) ) ;
#8396 = CARTESIAN_POINT ( 'NONE',  ( 70.21613547800127719, 6.123233995736675563E-16, -5.000000000000007994 ) ) ;
#8397 = ORIENTED_EDGE ( 'NONE', *, *, #22614, .F. ) ;
#8398 = CARTESIAN_POINT ( 'NONE',  ( 9.499999999999790390, 3.086737114213260025, -11.30674201446023019 ) ) ;
#8399 = CIRCLE ( 'NONE', #13074, 11.68650000001168898 ) ;
#8400 = AXIS2_PLACEMENT_3D ( 'NONE', #3903, #7423, #369 ) ;
#8401 = VERTEX_POINT ( 'NONE', #11429 ) ;
#8402 = ADVANCED_FACE ( 'NONE', ( #9254 ), #8275, .T. ) ;
#8403 = AXIS2_PLACEMENT_3D ( 'NONE', #14766, #5270, #1501 ) ;
#8404 = ORIENTED_EDGE ( 'NONE', *, *, #21020, .F. ) ;
#8405 = CARTESIAN_POINT ( 'NONE',  ( 7.685661446561619314, 5.583959896779020049, 6.259589141758143960 ) ) ;
#8406 = CARTESIAN_POINT ( 'NONE',  ( -5.871322893123450015, -8.081182679344781405, 10.50674201446023304 ) ) ;
#8407 = ORIENTED_EDGE ( 'NONE', *, *, #6902, .T. ) ;
#8408 = DIRECTION ( 'NONE',  ( 0.000000000000000000, -1.000000000000000000, 0.000000000000000000 ) ) ;
#8409 = DIRECTION ( 'NONE',  ( 0.000000000000000000, -1.000000000000000000, 0.000000000000000000 ) ) ;
#8410 = EDGE_CURVE ( 'NONE', #6680, #2307, #13344, .T. ) ;
#8411 = CARTESIAN_POINT ( 'NONE',  ( -1.504652183083727168, 9.499999999999904077, 2.610843423304989308 ) ) ;
#8412 = DIRECTION ( 'NONE',  ( 1.000000000000000000, 0.000000000000000000, 0.000000000000000000 ) ) ;
#8413 = ADVANCED_FACE ( 'NONE', ( #9719 ), #4148, .F. ) ;
#8414 = ORIENTED_EDGE ( 'NONE', *, *, #11688, .F. ) ;
#8415 = DIRECTION ( 'NONE',  ( 0.000000000000000000, 0.000000000000000000, 1.000000000000000000 ) ) ;
#8416 = CARTESIAN_POINT ( 'NONE',  ( -9.499999999999962697, -8.297908579805900909E-07, -3.500254135480583617 ) ) ;
#8417 = DIRECTION ( 'NONE',  ( -1.000000000000000000, -0.000000000000000000, -0.000000000000000000 ) ) ;
#8418 = ORIENTED_EDGE ( 'NONE', *, *, #14880, .T. ) ;
#8419 = VECTOR ( 'NONE', #23906, 1000.000000000000000 ) ;
#8420 = DIRECTION ( 'NONE',  ( 0.000000000000000000, 0.000000000000000000, 1.000000000000000000 ) ) ;
#8421 = ORIENTED_EDGE ( 'NONE', *, *, #6346, .F. ) ;
#8422 = CARTESIAN_POINT ( 'NONE',  ( 41.00000000000000000, 5.999999999999986677, 11.00000000000000000 ) ) ;
#8423 = LINE ( 'NONE', #6606, #13384 ) ;
#8424 = CARTESIAN_POINT ( 'NONE',  ( 0.000000000000000000, 45.00000000000000000, -27.00000000000000000 ) ) ;
#8425 = CARTESIAN_POINT ( 'NONE',  ( 41.73082370883260239, 27.62204025492843940, -1.500000000000000000 ) ) ;
#8426 = AXIS2_PLACEMENT_3D ( 'NONE', #21854, #18564, #12445 ) ;
#8427 = AXIS2_PLACEMENT_3D ( 'NONE', #8532, #19663, #2938 ) ;
#8428 = DIRECTION ( 'NONE',  ( -1.000000000000000000, 0.000000000000000000, 0.000000000000000000 ) ) ;
#8429 = ORIENTED_EDGE ( 'NONE', *, *, #13213, .F. ) ;
#8430 = DIRECTION ( 'NONE',  ( 0.000000000000000000, -0.000000000000000000, -1.000000000000000000 ) ) ;
#8431 = ORIENTED_EDGE ( 'NONE', *, *, #14831, .F. ) ;
#8432 = EDGE_CURVE ( 'NONE', #5616, #7931, #17377, .T. ) ;
#8433 = CARTESIAN_POINT ( 'NONE',  ( 42.00000000000000711, -26.82133436441677077, 11.58578643762690241 ) ) ;
#8434 = VERTEX_POINT ( 'NONE', #2419 ) ;
#8435 = CARTESIAN_POINT ( 'NONE',  ( -7.022953521755574080, 5.102474405759713783, 3.433165578109189209 ) ) ;
#8436 = VECTOR ( 'NONE', #15994, 1000.000000000000000 ) ;
#8437 = DIRECTION ( 'NONE',  ( 1.000000000000000000, 0.000000000000000000, 0.000000000000000000 ) ) ;
#8438 = ORIENTED_EDGE ( 'NONE', *, *, #19302, .T. ) ;
#8439 = EDGE_CURVE ( 'NONE', #8203, #3887, #11371, .T. ) ;
#8440 = CIRCLE ( 'NONE', #22101, 11.68650000001168721 ) ;
#8441 = CARTESIAN_POINT ( 'NONE',  ( -29.00000000000000000, -29.49999999999999645, 12.00000000000000000 ) ) ;
#8442 = ADVANCED_FACE ( 'NONE', ( #17540 ), #838, .T. ) ;
#8443 = CARTESIAN_POINT ( 'NONE',  ( -1.999999999999994449, -45.00000000000000000, 0.02500000000000418554 ) ) ;
#8444 = EDGE_CURVE ( 'NONE', #8229, #5720, #17429, .T. ) ;
#8445 = VERTEX_POINT ( 'NONE', #8395 ) ;
#8446 = VERTEX_POINT ( 'NONE', #4637 ) ;
#8447 = DIRECTION ( 'NONE',  ( 0.8571673007021120005, 1.049727191138618326E-16, -0.5150380749100547106 ) ) ;
#8448 = CARTESIAN_POINT ( 'NONE',  ( -9.500000000000000000, -6.482511860946779655E-13, -11.05958914175814556 ) ) ;
#8449 = ORIENTED_EDGE ( 'NONE', *, *, #6876, .T. ) ;
#8450 = VERTEX_POINT ( 'NONE', #10207 ) ;
#8451 = CARTESIAN_POINT ( 'NONE',  ( 31.49999999999999289, 50.99999999999999289, 12.50000000000000000 ) ) ;
#8452 = AXIS2_PLACEMENT_3D ( 'NONE', #9151, #3182, #10612 ) ;
#8453 = CARTESIAN_POINT ( 'NONE',  ( -1.999999999999994449, 45.00000000000000000, -23.99999999999999645 ) ) ;
#8454 = VERTEX_POINT ( 'NONE', #23177 ) ;
#8455 = DIRECTION ( 'NONE',  ( 1.000000000000000000, -0.000000000000000000, -0.000000000000000000 ) ) ;
#8456 = TOROIDAL_SURFACE ( 'NONE', #20936, 3.999999999999999112, 1.000000000000000000 ) ;
#8457 = ORIENTED_EDGE ( 'NONE', *, *, #7777, .F. ) ;
#8458 = CARTESIAN_POINT ( 'NONE',  ( -23.84999999999999432, -15.03999999999999915, -27.00000000000000000 ) ) ;
#8459 = CARTESIAN_POINT ( 'NONE',  ( 33.99999999999998579, -1.387778780781445676E-14, 11.00000000000000000 ) ) ;
#8460 = PRODUCT_DEFINITION_SHAPE ( 'NONE', 'NONE',  #24106 ) ;
#8461 = FACE_OUTER_BOUND ( 'NONE', #3312, .T. ) ;
#8462 = CARTESIAN_POINT ( 'NONE',  ( 62.94340820527399671, -1.078520768856852078E-29, 5.000000000000007994 ) ) ;
#8463 = EDGE_CURVE ( 'NONE', #2741, #18301, #20779, .T. ) ;
#8464 = LINE ( 'NONE', #2618, #5652 ) ;
#8465 = EDGE_LOOP ( 'NONE', ( #9544, #12396 ) ) ;
#8466 = DIRECTION ( 'NONE',  ( 1.000000000000000000, -2.600433232233976523E-16, 0.000000000000000000 ) ) ;
#8467 = DIRECTION ( 'NONE',  ( -0.000000000000000000, -0.000000000000000000, -1.000000000000000000 ) ) ;
#8468 = CARTESIAN_POINT ( 'NONE',  ( -23.89999999999999858, 29.50000000000000000, -27.00000000000000000 ) ) ;
#8469 = CARTESIAN_POINT ( 'NONE',  ( 9.499999999999790390, 3.086737114213260025, 8.159589141758143427 ) ) ;
#8470 = EDGE_CURVE ( 'NONE', #5783, #4077, #18449, .T. ) ;
#8471 = ORIENTED_EDGE ( 'NONE', *, *, #5084, .T. ) ;
#8472 = ORIENTED_EDGE ( 'NONE', *, *, #20878, .F. ) ;
#8473 = EDGE_CURVE ( 'NONE', #411, #22901, #23421, .T. ) ;
#8474 = EDGE_CURVE ( 'NONE', #21978, #6073, #22672, .T. ) ;
#8475 = FACE_OUTER_BOUND ( 'NONE', #18269, .T. ) ;
#8476 = CARTESIAN_POINT ( 'NONE',  ( -14.79187224938324974, -2.570168443617189880, -9.168425918763428939 ) ) ;
#8477 = CARTESIAN_POINT ( 'NONE',  ( 29.00000000000000000, 29.50000000000000355, 11.00000000000000000 ) ) ;
#8478 = ORIENTED_EDGE ( 'NONE', *, *, #11142, .F. ) ;
#8479 = CARTESIAN_POINT ( 'NONE',  ( 39.00000000000000000, 0.000000000000000000, 12.00000000000000000 ) ) ;
#8480 = CYLINDRICAL_SURFACE ( 'NONE', #2713, 5.000000000000000888 ) ;
#8481 = VERTEX_POINT ( 'NONE', #14017 ) ;
#8482 = DIRECTION ( 'NONE',  ( 1.000000000000000000, -0.000000000000000000, -0.000000000000000000 ) ) ;
#8483 = FACE_OUTER_BOUND ( 'NONE', #10002, .T. ) ;
#8484 = CARTESIAN_POINT ( 'NONE',  ( -7.685661446561619314, -5.583959896779019161, 6.406742014460233392 ) ) ;
#8485 = EDGE_CURVE ( 'NONE', #19575, #7696, #13903, .T. ) ;
#8486 = VERTEX_POINT ( 'NONE', #19509 ) ;
#8487 = DIRECTION ( 'NONE',  ( -1.000000000000000000, 0.000000000000000000, 0.000000000000000000 ) ) ;
#8488 = CARTESIAN_POINT ( 'NONE',  ( 9.500000000000000000, 6.470877716354879437E-13, 4.059589141758143782 ) ) ;
#8489 = AXIS2_PLACEMENT_3D ( 'NONE', #1796, #14290, #16546 ) ;
#8490 = CARTESIAN_POINT ( 'NONE',  ( 63.23840997654417606, 6.123233995736675563E-16, -5.000000000000007994 ) ) ;
#8491 = CYLINDRICAL_SURFACE ( 'NONE', #22420, 5.100000000000000533 ) ;
#8492 = EDGE_CURVE ( 'NONE', #23530, #21399, #9844, .T. ) ;
#8493 = CARTESIAN_POINT ( 'NONE',  ( -2.682529543899159208, -8.255977015246598327, -10.03316557810918930 ) ) ;
#8494 = CARTESIAN_POINT ( 'NONE',  ( 84.18181818181818699, -4.172000000000000597, 0.000000000000000000 ) ) ;
#8495 = VERTEX_POINT ( 'NONE', #972 ) ;
#8496 = ORIENTED_EDGE ( 'NONE', *, *, #21946, .F. ) ;
#8497 = EDGE_CURVE ( 'NONE', #13580, #1785, #21462, .T. ) ;
#8498 = CARTESIAN_POINT ( 'NONE',  ( 5.365059087798938364, 7.384370330707087149, 4.933165578109187877 ) ) ;
#8499 = ADVANCED_FACE ( 'NONE', ( #727 ), #4755, .F. ) ;
#8500 = ORIENTED_EDGE ( 'NONE', *, *, #19851, .T. ) ;
#8501 = DIRECTION ( 'NONE',  ( -0.8589545652107374307, -0.5120518088080863173, -8.326672684688674053E-17 ) ) ;
#8502 = DIRECTION ( 'NONE',  ( 1.000000000000000000, 0.000000000000000000, 0.000000000000000000 ) ) ;
#8503 = ORIENTED_EDGE ( 'NONE', *, *, #7354, .F. ) ;
#8504 = CARTESIAN_POINT ( 'NONE',  ( 30.44534269664589843, 40.40463133211081015, -27.00000000000000000 ) ) ;
#8505 = CARTESIAN_POINT ( 'NONE',  ( 2.935661446562616295, -9.035036904803758873, -5.659589141758144315 ) ) ;
#8506 = VECTOR ( 'NONE', #11391, 1000.000000000000000 ) ;
#8507 = CIRCLE ( 'NONE', #22939, 9.499999999999989342 ) ;
#8508 = CARTESIAN_POINT ( 'NONE',  ( -2.903219370115622588, 8.518977561982945090, 99.78095984017566877 ) ) ;
#8509 = CARTESIAN_POINT ( 'NONE',  ( -2.935661446562617183, 9.035036904803758873, 3.806742014460233303 ) ) ;
#8510 = CARTESIAN_POINT ( 'NONE',  ( 0.000000000000000000, 45.00000000000000000, -27.00000000000000000 ) ) ;
#8511 = ORIENTED_EDGE ( 'NONE', *, *, #5103, .F. ) ;
#8512 = CARTESIAN_POINT ( 'NONE',  ( -31.50000000000001421, 50.99999999999999289, 12.50000000000000000 ) ) ;
#8513 = CARTESIAN_POINT ( 'NONE',  ( 0.000000000000000000, -12.99147757894464306, 7.750000000000000000 ) ) ;
#8514 = AXIS2_PLACEMENT_3D ( 'NONE', #20216, #7145, #14450 ) ;
#8515 = CARTESIAN_POINT ( 'NONE',  ( 58.57977184163763695, 7.562528597612068045E-15, 0.000000000000000000 ) ) ;
#8516 = ORIENTED_EDGE ( 'NONE', *, *, #14406, .T. ) ;
#8517 = DIRECTION ( 'NONE',  ( -1.000000000000000000, 0.000000000000000000, 0.000000000000000000 ) ) ;
#8518 = CARTESIAN_POINT ( 'NONE',  ( 11.50000000000000000, 2.967071445749915437, 17.62702788437274393 ) ) ;
#8519 = CARTESIAN_POINT ( 'NONE',  ( 24.75000000000000711, -29.50000000000000000, 12.50000000000000000 ) ) ;
#8520 = EDGE_CURVE ( 'NONE', #1759, #13616, #10248, .T. ) ;
#8521 = ORIENTED_EDGE ( 'NONE', *, *, #8641, .F. ) ;
#8522 = CARTESIAN_POINT ( 'NONE',  ( 2.682529543899157876, 8.255977015246598327, -5.033165578109189298 ) ) ;
#8523 = VERTEX_POINT ( 'NONE', #17305 ) ;
#8524 = ORIENTED_EDGE ( 'NONE', *, *, #18792, .T. ) ;
#8525 = CARTESIAN_POINT ( 'NONE',  ( 5.871322893123449127, 8.081182679344781405, 6.359589141758142716 ) ) ;
#8526 = CARTESIAN_POINT ( 'NONE',  ( 2.935661446562616295, -9.035036904803758873, 4.806742014460232859 ) ) ;
#8527 = ORIENTED_EDGE ( 'NONE', *, *, #3191, .F. ) ;
#8528 = CARTESIAN_POINT ( 'NONE',  ( 11.50000000000000000, 2.967071445750145919, -17.62702788437270840 ) ) ;
#8529 = CARTESIAN_POINT ( 'NONE',  ( 23.85000000000000142, 15.03999999999999737, 2.200000000000000178 ) ) ;
#8530 = CARTESIAN_POINT ( 'NONE',  ( -9.500000000000211386, 3.086737114211961064, 6.959589141758143249 ) ) ;
#8531 = CIRCLE ( 'NONE', #21003, 3.000000000000002665 ) ;
#8532 = CARTESIAN_POINT ( 'NONE',  ( -41.00000000000000000, -4.000000000000000888, 10.49999999999999822 ) ) ;
#8533 = CARTESIAN_POINT ( 'NONE',  ( 35.99999999999999289, 50.99999999999999289, 0.5000000000000000000 ) ) ;
#8534 = PRODUCT_DEFINITION ( 'UNKNOWN', '', #5716, #11865 ) ;
#8535 = DIRECTION ( 'NONE',  ( -4.613626265895764052E-16, -1.000000000000000000, 0.000000000000000000 ) ) ;
#8536 = VERTEX_POINT ( 'NONE', #608 ) ;
#8537 = DIRECTION ( 'NONE',  ( 0.7071067811865660024, 8.659560562355159656E-17, -0.7071067811865291430 ) ) ;
#8538 = LINE ( 'NONE', #8047, #10225 ) ;
#8539 = DIRECTION ( 'NONE',  ( 1.000000000000000000, 0.000000000000000000, 0.000000000000000000 ) ) ;
#8540 = PLANE ( 'NONE',  #795 ) ;
#8541 = ADVANCED_FACE ( 'NONE', ( #2670 ), #21082, .T. ) ;
#8542 = VERTEX_POINT ( 'NONE', #10086 ) ;
#8543 = ADVANCED_FACE ( 'NONE', ( #8135 ), #21581, .T. ) ;
#8544 = DIRECTION ( 'NONE',  ( 0.000000000000000000, 1.000000000000000000, 0.000000000000000000 ) ) ;
#8545 = VERTEX_POINT ( 'NONE', #20229 ) ;
#8546 = DIRECTION ( 'NONE',  ( 1.000000000000000000, 0.000000000000000000, 0.000000000000000000 ) ) ;
#8547 = ORIENTED_EDGE ( 'NONE', *, *, #9876, .T. ) ;
#8548 = AXIS2_PLACEMENT_3D ( 'NONE', #4047, #505, #22846 ) ;
#8549 = CARTESIAN_POINT ( 'NONE',  ( 5.365059087798939252, 7.384370330707087149, 4.933165578109186988 ) ) ;
#8550 = CARTESIAN_POINT ( 'NONE',  ( 81.85249911436491743, 7.562528597612068045E-15, 0.000000000000000000 ) ) ;
#8551 = DIRECTION ( 'NONE',  ( -0.000000000000000000, -0.000000000000000000, -1.000000000000000000 ) ) ;
#8552 = LINE ( 'NONE', #15997, #19347 ) ;
#8553 = CARTESIAN_POINT ( 'NONE',  ( 71.67068093254673045, 7.562528597612068045E-15, 0.000000000000000000 ) ) ;
#8554 = CARTESIAN_POINT ( 'NONE',  ( -2.024999999999999911, -45.00000000000000000, 27.00000000000000000 ) ) ;
#8555 = EDGE_CURVE ( 'NONE', #22930, #1008, #20006, .T. ) ;
#8556 = CARTESIAN_POINT ( 'NONE',  ( -9.500000000000211386, 3.086737114211961064, -6.106742014460234458 ) ) ;
#8557 = ORIENTED_EDGE ( 'NONE', *, *, #6282, .F. ) ;
#8558 = EDGE_LOOP ( 'NONE', ( #13973, #20598, #10622, #21811 ) ) ;
#8559 = CARTESIAN_POINT ( 'NONE',  ( -9.363405990316115535, -0.7769257075329323303, -12.13659400968388269 ) ) ;
#8560 = AXIS2_PLACEMENT_3D ( 'NONE', #1239, #12066, #16110 ) ;
#8561 = ORIENTED_EDGE ( 'NONE', *, *, #5963, .F. ) ;
#8562 = LINE ( 'NONE', #1033, #14737 ) ;
#8563 = ADVANCED_FACE ( 'NONE', ( #23882 ), #12413, .T. ) ;
#8564 = EDGE_CURVE ( 'NONE', #9329, #14658, #12136, .T. ) ;
#8565 = ORIENTED_EDGE ( 'NONE', *, *, #21568, .F. ) ;
#8566 = LINE ( 'NONE', #16011, #3695 ) ;
#8567 = ADVANCED_FACE ( 'NONE', ( #10570 ), #1638, .T. ) ;
#8568 = DIRECTION ( 'NONE',  ( 0.000000000000000000, 0.2817325568414237313, 0.9594929736144991450 ) ) ;
#8569 = ADVANCED_FACE ( 'NONE', ( #3505 ), #12515, .T. ) ;
#8570 = CARTESIAN_POINT ( 'NONE',  ( -34.00000000000000000, -3.851859888774471706E-31, 9.500000000000000000 ) ) ;
#8571 = DIRECTION ( 'NONE',  ( 0.000000000000000000, 0.000000000000000000, 1.000000000000000000 ) ) ;
#8572 = DIRECTION ( 'NONE',  ( 0.000000000000000000, 0.000000000000000000, 1.000000000000000000 ) ) ;
#8573 = ORIENTED_EDGE ( 'NONE', *, *, #9196, .T. ) ;
#8574 = CARTESIAN_POINT ( 'NONE',  ( 79.81818181818181301, 7.491529369508391930E-15, 0.000000000000000000 ) ) ;
#8575 = DIRECTION ( 'NONE',  ( -0.000000000000000000, -0.000000000000000000, -1.000000000000000000 ) ) ;
#8576 = CARTESIAN_POINT ( 'NONE',  ( -6.153822176767817416E-13, 9.500000000000000000, 2.559589141758142894 ) ) ;
#8577 = CARTESIAN_POINT ( 'NONE',  ( 9.500000000000209610, -3.086737114211962396, 5.959589141758143249 ) ) ;
#8578 = CIRCLE ( 'NONE', #12867, 9.000000000000000000 ) ;
#8579 = CARTESIAN_POINT ( 'NONE',  ( -34.00000000000000000, -4.999999999999999112, 11.00000000000000000 ) ) ;
#8580 = CARTESIAN_POINT ( 'NONE',  ( -28.27483331787888332, -41.23752903419610050, 12.00000000000000000 ) ) ;
#8581 = EDGE_CURVE ( 'NONE', #6008, #22050, #10627, .T. ) ;
#8582 = CARTESIAN_POINT ( 'NONE',  ( -7.999999999999992895, 0.000000000000000000, 105.0000000000000000 ) ) ;
#8583 = ORIENTED_EDGE ( 'NONE', *, *, #16821, .T. ) ;
#8584 = CARTESIAN_POINT ( 'NONE',  ( -17.38700629636781869, -8.908123924593986942, 3.336041480784321500 ) ) ;
#8585 = DIRECTION ( 'NONE',  ( 0.000000000000000000, -1.000000000000000000, 0.000000000000000000 ) ) ;
#8586 = CARTESIAN_POINT ( 'NONE',  ( 23.00000000000000000, 11.58003564732003277, -1.573866785045813010 ) ) ;
#8587 = EDGE_LOOP ( 'NONE', ( #21671, #23043, #23181, #24067 ) ) ;
#8588 = CYLINDRICAL_SURFACE ( 'NONE', #10354, 8.000000000000003553 ) ;
#8589 = DIRECTION ( 'NONE',  ( 0.4011779117250717785, -0.9160001545545232160, 0.000000000000000000 ) ) ;
#8590 = CARTESIAN_POINT ( 'NONE',  ( 2.935661446562616295, -9.035036904803758873, 4.806742014460232859 ) ) ;
#8591 = TOROIDAL_SURFACE ( 'NONE', #8985, 3.500000000000001776, 1.500000000000000000 ) ;
#8592 = EDGE_CURVE ( 'NONE', #23710, #15773, #2067, .T. ) ;
#8593 = CARTESIAN_POINT ( 'NONE',  ( 0.000000000000000000, 45.00000000000000000, -27.00000000000000000 ) ) ;
#8594 = EDGE_CURVE ( 'NONE', #12158, #7578, #14601, .T. ) ;
#8595 = DIRECTION ( 'NONE',  ( -0.8428161139095668997, 0.000000000000000000, 0.5382016333442104505 ) ) ;
#8596 = CARTESIAN_POINT ( 'NONE',  ( 17.19784311473119587, -8.411123426659415259, -4.422670359120409955 ) ) ;
#8597 = LINE ( 'NONE', #2647, #2130 ) ;
#8598 = CARTESIAN_POINT ( 'NONE',  ( -7.022953521755574080, 5.102474405759713783, -3.433165578109189209 ) ) ;
#8599 = EDGE_LOOP ( 'NONE', ( #2124, #1975, #6499, #3837, #23313, #22165 ) ) ;
#8600 = DIRECTION ( 'NONE',  ( -0.000000000000000000, -0.000000000000000000, -1.000000000000000000 ) ) ;
#8601 = ORIENTED_EDGE ( 'NONE', *, *, #1950, .F. ) ;
#8602 = CARTESIAN_POINT ( 'NONE',  ( -8.680847955711007202, -5.923547351154968927E-13, 7.633165578109188942 ) ) ;
#8603 = ORIENTED_EDGE ( 'NONE', *, *, #11375, .T. ) ;
#8604 = APPLICATION_PROTOCOL_DEFINITION ( 'draft international standard', 'automotive_design', 1998, #22721 ) ;
#8605 =( BOUNDED_CURVE ( )  B_SPLINE_CURVE ( 2, ( #9337, #14955, #16782, #22653, #100, #22433, #13134, #17149, #2028, #9454, #7633, #15074, #22544, #5819, #17035, #5937, #6670, #4494, #9809, #14099, #13993, #11649, #10318, #17779, #1070, #23153, #8493, #2759, #19117, #11901, #17277, #4238, #21437, #8366, #15556, #4726, #19486, #10060, #9945, #10178, #2391, #12131, #943, #4612, #577, #19374, #12014, #19609, #7998, #15935, #2889, #17635, #23400, #4357, #701, #17514, #13877, #15446, #6435, #21321, #15818, #22909, #6185, #13621, #2648, #8227, #21061, #8110, #11764, #17406, #19245, #2524, #23020, #23283, #6293, #13739, #21190, #816, #15678, #6557, #5077, #14441, #10437, #3018, #14335, #6914, #1437, #17898, #8848, #3365, #23508, #8954, #8598, #18140, #21683, #14571, #4977 ),
 .UNSPECIFIED., .F., .F. ) 
 B_SPLINE_CURVE_WITH_KNOTS ( ( 3, 2, 2, 2, 2, 2, 2, 2, 2, 2, 2, 2, 2, 2, 2, 2, 2, 2, 2, 2, 2, 2, 2, 2, 2, 2, 2, 2, 2, 2, 2, 2, 2, 2, 2, 2, 2, 2, 2, 2, 2, 2, 2, 2, 2, 2, 2, 2, 3 ),
 ( 0.01324393663734964137, 0.02000000000000000042, 0.04000000000000000083, 0.05999999999999999778, 0.08000000000000000167, 0.1000000000000000056, 0.1199999999999999956, 0.1400000000000000133, 0.1600000000000000033, 0.1799999999999999933, 0.2000000000000000111, 0.2200000000000000011, 0.2399999999999999911, 0.2600000000000000644, 0.2800000000000000266, 0.2999999999999999889, 0.3200000000000000067, 0.3400000000000000244, 0.3599999999999999867, 0.3799999999999999489, 0.4000000000000000222, 0.4199999999999999845, 0.4400000000000000022, 0.4600000000000000200, 0.4799999999999999822, 0.5000000000000000000, 0.5200000000000000178, 0.5400000000000000355, 0.5600000000000000533, 0.5799999999999999600, 0.5999999999999999778, 0.6199999999999998845, 0.6400000000000000133, 0.6600000000000000311, 0.6800000000000000488, 0.6999999999999999556, 0.7199999999999999734, 0.7399999999999999911, 0.7600000000000000089, 0.7800000000000000266, 0.8000000000000001554, 0.8199999999999999512, 0.8399999999999999689, 0.8599999999999999867, 0.8800000000000000044, 0.9000000000000000222, 0.9200000000000000400, 0.9399999999999998357, 0.9500000000000000666 ),
 .UNSPECIFIED. ) 
 CURVE ( )  GEOMETRIC_REPRESENTATION_ITEM ( )  RATIONAL_B_SPLINE_CURVE ( ( 0.9781034501096599332, 0.9834667361450606382, 1.000000000000000000, 0.9510565162951535312, 1.000000000000000000, 0.9510565162951535312, 1.000000000000000000, 0.9510565162951535312, 1.000000000000000000, 0.9510565162951535312, 1.000000000000000000, 0.9510565162951535312, 1.000000000000000000, 0.9510565162951535312, 1.000000000000000000, 0.9510565162951535312, 1.000000000000000000, 0.9510565162951535312, 1.000000000000000000, 0.9510565162951535312, 1.000000000000000000, 0.9510565162951535312, 1.000000000000000000, 0.9510565162951535312, 1.000000000000000000, 0.9510565162951535312, 1.000000000000000000, 0.9510565162951535312, 1.000000000000000000, 0.9510565162951535312, 1.000000000000000000, 0.9510565162951535312, 1.000000000000000000, 0.9510565162951535312, 1.000000000000000000, 0.9510565162951535312, 1.000000000000000000, 0.9510565162951535312, 1.000000000000000000, 0.9510565162951535312, 1.000000000000000000, 0.9510565162951535312, 1.000000000000000000, 0.9510565162951535312, 1.000000000000000000, 0.9510565162951535312, 1.000000000000000000, 0.9510565162951535312, 1.000000000000000000, 0.9510565162951535312, 1.000000000000000000, 0.9510565162951535312, 1.000000000000000000, 0.9510565162951535312, 1.000000000000000000, 0.9510565162951535312, 1.000000000000000000, 0.9510565162951535312, 1.000000000000000000, 0.9510565162951535312, 1.000000000000000000, 0.9510565162951535312, 1.000000000000000000, 0.9510565162951535312, 1.000000000000000000, 0.9510565162951535312, 1.000000000000000000, 0.9510565162951535312, 1.000000000000000000, 0.9510565162951535312, 1.000000000000000000, 0.9510565162951535312, 1.000000000000000000, 0.9510565162951535312, 1.000000000000000000, 0.9510565162951535312, 1.000000000000000000, 0.9510565162951535312, 1.000000000000000000, 0.9510565162951535312, 1.000000000000000000, 0.9510565162951535312, 1.000000000000000000, 0.9510565162951535312, 1.000000000000000000, 0.9510565162951535312, 1.000000000000000000, 0.9510565162951535312, 1.000000000000000000, 0.9510565162951535312, 1.000000000000000000, 0.9510565162951535312, 1.000000000000000000, 0.9510565162951535312, 1.000000000000000000, 0.9755282581475764880, 0.9755282581475768211 ) ) 
 REPRESENTATION_ITEM ( '' )  );
#8606 = DIRECTION ( 'NONE',  ( 0.000000000000000000, -1.000000000000000000, 0.000000000000000000 ) ) ;
#8607 = VECTOR ( 'NONE', #19294, 1000.000000000000000 ) ;
#8608 = ORIENTED_EDGE ( 'NONE', *, *, #294, .F. ) ;
#8609 = EDGE_LOOP ( 'NONE', ( #15670, #17063, #24069, #11580 ) ) ;
#8610 = DIRECTION ( 'NONE',  ( -1.000000000000000000, 0.000000000000000000, 0.000000000000000000 ) ) ;
#8611 = CARTESIAN_POINT ( 'NONE',  ( -6.822232771736903637E-13, 9.988891130263535700, -4.559589141758142894 ) ) ;
#8612 = UNCERTAINTY_MEASURE_WITH_UNIT (LENGTH_MEASURE( 1.000000000000000082E-05 ), #22086, 'distance_accuracy_value', 'NONE');
#8613 = DIRECTION ( 'NONE',  ( 0.000000000000000000, 0.000000000000000000, 1.000000000000000000 ) ) ;
#8614 = LINE ( 'NONE', #7277, #12317 ) ;
#8615 = DIRECTION ( 'NONE',  ( 1.000000000000000000, 0.000000000000000000, 0.000000000000000000 ) ) ;
#8616 = DIRECTION ( 'NONE',  ( 1.049727191138618449E-16, -0.5150380749100544886, 0.8571673007021121116 ) ) ;
#8617 = DIRECTION ( 'NONE',  ( 0.000000000000000000, 0.000000000000000000, -1.000000000000000000 ) ) ;
#8618 = DIRECTION ( 'NONE',  ( 4.613626265895763066E-16, 1.000000000000000000, 0.000000000000000000 ) ) ;
#8619 = EDGE_CURVE ( 'NONE', #208, #2307, #1681, .T. ) ;
#8620 = DIRECTION ( 'NONE',  ( 1.000000000000000000, 0.000000000000000000, -0.000000000000000000 ) ) ;
#8621 = CARTESIAN_POINT ( 'NONE',  ( 82.14750088563508257, 6.123233995736675563E-16, -5.000000000000007994 ) ) ;
#8622 = CIRCLE ( 'NONE', #17981, 4.172000000000008590 ) ;
#8623 = CARTESIAN_POINT ( 'NONE',  ( 0.000000000000000000, -45.00000000000000000, 23.99999999999999645 ) ) ;
#8624 = VERTEX_POINT ( 'NONE', #8621 ) ;
#8625 = CONICAL_SURFACE ( 'NONE', #15281, 0.7000000000000005107, 0.7853981633974458365 ) ;
#8626 = CARTESIAN_POINT ( 'NONE',  ( 9.500000000000209610, -3.086737114211962396, -13.10674201446023091 ) ) ;
#8627 = AXIS2_PLACEMENT_3D ( 'NONE', #7012, #11241, #1430 ) ;
#8628 = ORIENTED_EDGE ( 'NONE', *, *, #12440, .F. ) ;
#8629 = VERTEX_POINT ( 'NONE', #16074 ) ;
#8630 = CARTESIAN_POINT ( 'NONE',  ( -9.499999999999790390, -3.086737114213257804, 5.159589141758141650 ) ) ;
#8631 = CARTESIAN_POINT ( 'NONE',  ( 7.685661446561619314, 5.583959896779020049, 9.406742014460235168 ) ) ;
#8632 = ORIENTED_EDGE ( 'NONE', *, *, #18850, .F. ) ;
#8633 = CARTESIAN_POINT ( 'NONE',  ( -43.50000000000001421, 50.99999999999995026, 0.000000000000000000 ) ) ;
#8634 = DIRECTION ( 'NONE',  ( 0.000000000000000000, 0.000000000000000000, -1.000000000000000000 ) ) ;
#8635 = CARTESIAN_POINT ( 'NONE',  ( 62.94340820527399671, 7.562528597612068045E-15, 0.000000000000000000 ) ) ;
#8636 = DIRECTION ( 'NONE',  ( -1.000000000000000000, -1.224606353822377258E-16, -0.000000000000000000 ) ) ;
#8637 = EDGE_CURVE ( 'NONE', #14695, #19097, #22729, .T. ) ;
#8638 = AXIS2_PLACEMENT_3D ( 'NONE', #3164, #21839, #8535 ) ;
#8639 = DIRECTION ( 'NONE',  ( -0.000000000000000000, -0.000000000000000000, -1.000000000000000000 ) ) ;
#8640 = LINE ( 'NONE', #19664, #23859 ) ;
#8641 = EDGE_CURVE ( 'NONE', #18942, #1347, #21818, .T. ) ;
#8642 = AXIS2_PLACEMENT_3D ( 'NONE', #23443, #15871, #6601 ) ;
#8643 = PRODUCT_DEFINITION_SHAPE ( 'NONE', 'NONE',  #13603 ) ;
#8644 = CIRCLE ( 'NONE', #18015, 1.000000000000000888 ) ;
#8645 = VECTOR ( 'NONE', #9410, 1000.000000000000000 ) ;
#8646 = ADVANCED_FACE ( 'NONE', ( #19987 ), #8296, .F. ) ;
#8647 = ORIENTED_EDGE ( 'NONE', *, *, #6530, .F. ) ;
#8648 = ADVANCED_FACE ( 'NONE', ( #10695 ), #1462, .F. ) ;
#8649 = ORIENTED_EDGE ( 'NONE', *, *, #4829, .F. ) ;
#8650 = DIRECTION ( 'NONE',  ( -0.000000000000000000, 0.000000000000000000, -1.000000000000000000 ) ) ;
#8651 = CARTESIAN_POINT ( 'NONE',  ( -40.23082370883257397, -29.50000000000000711, -1.500000000000000000 ) ) ;
#8652 = CARTESIAN_POINT ( 'NONE',  ( 0.000000000000000000, 0.000000000000000000, 12.50000000000000000 ) ) ;
#8653 = DIRECTION ( 'NONE',  ( -0.000000000000000000, -0.000000000000000000, 1.000000000000000000 ) ) ;
#8654 = ORIENTED_EDGE ( 'NONE', *, *, #1753, .T. ) ;
#8655 = CARTESIAN_POINT ( 'NONE',  ( 9.500000000000000000, 6.470877716354879437E-13, 8.059589141758143782 ) ) ;
#8656 = ORIENTED_EDGE ( 'NONE', *, *, #1014, .T. ) ;
#8657 = CARTESIAN_POINT ( 'NONE',  ( 7.685661446561619314, 5.583959896779020049, -6.259589141758143960 ) ) ;
#8658 = ORIENTED_EDGE ( 'NONE', *, *, #23643, .T. ) ;
#8659 = AXIS2_PLACEMENT_3D ( 'NONE', #10082, #5837, #242 ) ;
#8660 = CARTESIAN_POINT ( 'NONE',  ( -6.233975306307045953E-13, 9.127583699786111282, 5.133165578109188054 ) ) ;
#8661 = VECTOR ( 'NONE', #9022, 1000.000000000000000 ) ;
#8662 = AXIS2_PLACEMENT_3D ( 'NONE', #12159, #19985, #4881 ) ;
#8663 = VECTOR ( 'NONE', #18297, 1000.000000000000000 ) ;
#8664 = ORIENTED_EDGE ( 'NONE', *, *, #14514, .T. ) ;
#8665 = CARTESIAN_POINT ( 'NONE',  ( 63.81818181818181301, 7.491529369508391930E-15, 0.000000000000000000 ) ) ;
#8666 = CIRCLE ( 'NONE', #16840, 4.999999999999997335 ) ;
#8667 = DIRECTION ( 'NONE',  ( 0.000000000000000000, 0.000000000000000000, 1.000000000000000000 ) ) ;
#8668 = LINE ( 'NONE', #22973, #7096 ) ;
#8669 = VECTOR ( 'NONE', #22596, 1000.000000000000000 ) ;
#8670 = DIRECTION ( 'NONE',  ( -1.000000000000000000, 0.000000000000000000, 0.000000000000000000 ) ) ;
#8671 = EDGE_CURVE ( 'NONE', #1091, #6942, #23770, .T. ) ;
#8672 = ADVANCED_FACE ( 'NONE', ( #20117 ), #3393, .T. ) ;
#8673 = DIRECTION ( 'NONE',  ( 0.000000000000000000, 0.000000000000000000, -1.000000000000000000 ) ) ;
#8674 = EDGE_CURVE ( 'NONE', #15584, #6803, #11394, .T. ) ;
#8675 = CARTESIAN_POINT ( 'NONE',  ( 7.685661446561619314, 5.583959896779020049, -5.406742014460233392 ) ) ;
#8676 = ORIENTED_EDGE ( 'NONE', *, *, #17904, .F. ) ;
#8677 = ORIENTED_EDGE ( 'NONE', *, *, #11026, .T. ) ;
#8678 = CARTESIAN_POINT ( 'NONE',  ( -0.9343984967527667607, -9.063981491316820183, -12.39613733928520567 ) ) ;
#8679 = AXIS2_PLACEMENT_3D ( 'NONE', #11641, #18865, #17266 ) ;
#8680 = AXIS2_PLACEMENT_3D ( 'NONE', #15203, #3654, #2305 ) ;
#8681 = FACE_OUTER_BOUND ( 'NONE', #8116, .T. ) ;
#8682 = VECTOR ( 'NONE', #22253, 1000.000000000000000 ) ;
#8683 = CARTESIAN_POINT ( 'NONE',  ( 64.39795365981944997, -1.078520768856852078E-29, 5.000000000000007994 ) ) ;
#8684 = AXIS2_PLACEMENT_3D ( 'NONE', #19957, #19739, #21796 ) ;
#8685 = AXIS2_PLACEMENT_3D ( 'NONE', #5745, #3901, #5263 ) ;
#8686 = ORIENTED_EDGE ( 'NONE', *, *, #8170, .T. ) ;
#8687 = VECTOR ( 'NONE', #22316, 1000.000000000000000 ) ;
#8688 = CARTESIAN_POINT ( 'NONE',  ( 87.09090909090909349, -4.172000000000000597, 5.616230220889771312E-16 ) ) ;
#8689 = FACE_OUTER_BOUND ( 'NONE', #6166, .T. ) ;
#8690 = EDGE_LOOP ( 'NONE', ( #8157, #19943, #20750, #14632 ) ) ;
#8691 = DIRECTION ( 'NONE',  ( -0.000000000000000000, -0.000000000000000000, 1.000000000000000000 ) ) ;
#8692 = DIRECTION ( 'NONE',  ( 1.000000000000000000, 0.000000000000000000, 0.000000000000000000 ) ) ;
#8693 = FACE_OUTER_BOUND ( 'NONE', #20865, .T. ) ;
#8694 = PRODUCT_DEFINITION ( 'UNKNOWN', '', #22076, #13837 ) ;
#8695 = CARTESIAN_POINT ( 'NONE',  ( -41.99999999999999289, 25.93535998569253920, -27.00000000000000000 ) ) ;
#8696 = ADVANCED_FACE ( 'NONE', ( #5713 ), #20588, .F. ) ;
#8697 = PRESENTATION_LAYER_ASSIGNMENT (  '', '', ( #5989 ) ) ;
#8698 = ORIENTED_EDGE ( 'NONE', *, *, #2826, .T. ) ;
#8699 = AXIS2_PLACEMENT_3D ( 'NONE', #4943, #21148, #14072 ) ;
#8700 = VERTEX_POINT ( 'NONE', #2023 ) ;
#8701 = AXIS2_PLACEMENT_3D ( 'NONE', #6529, #7828, #4209 ) ;
#8702 = ADVANCED_FACE ( 'NONE', ( #4116 ), #1805, .F. ) ;
#8703 = VECTOR ( 'NONE', #13058, 1000.000000000000000 ) ;
#8704 = CIRCLE ( 'NONE', #4444, 5.000000000000007994 ) ;
#8705 = ORIENTED_EDGE ( 'NONE', *, *, #10905, .T. ) ;
#8706 = EDGE_CURVE ( 'NONE', #19009, #2972, #16102, .T. ) ;
#8707 = ORIENTED_EDGE ( 'NONE', *, *, #7307, .F. ) ;
#8708 = DIRECTION ( 'NONE',  ( 0.000000000000000000, -1.000000000000000000, 0.000000000000000000 ) ) ;
#8709 = EDGE_CURVE ( 'NONE', #9227, #2790, #7630, .T. ) ;
#8710 = AXIS2_PLACEMENT_3D ( 'NONE', #15460, #13389, #20854 ) ;
#8711 = CARTESIAN_POINT ( 'NONE',  ( 33.99999999999998579, 5.999999999999985789, 11.00000000000000000 ) ) ;
#8712 = DIRECTION ( 'NONE',  ( -1.000000000000000000, 0.000000000000000000, 0.000000000000000000 ) ) ;
#8713 = VERTEX_POINT ( 'NONE', #14829 ) ;
#8714 = CARTESIAN_POINT ( 'NONE',  ( -17.32141611691247718, -8.728455122802975197, 3.780491077225288432 ) ) ;
#8715 = CARTESIAN_POINT ( 'NONE',  ( -1.029124893018731811E-15, -45.00000000000000000, 22.79827876194487857 ) ) ;
#8716 = ORIENTED_EDGE ( 'NONE', *, *, #20366, .T. ) ;
#8717 = CARTESIAN_POINT ( 'NONE',  ( -0.9830802669677229932, 45.00000000000000000, 0.02500000000000418554 ) ) ;
#8718 = CARTESIAN_POINT ( 'NONE',  ( 29.00000000000000000, 29.50000000000000000, -3.000000000000000000 ) ) ;
#8719 = CARTESIAN_POINT ( 'NONE',  ( 20.85000000000000497, 15.03999999999999737, 2.200000000000000178 ) ) ;
#8720 = DIRECTION ( 'NONE',  ( 0.000000000000000000, -1.000000000000000000, 0.000000000000000000 ) ) ;
#8721 = DIRECTION ( 'NONE',  ( 0.000000000000000000, -1.000000000000000000, 9.256405414277000802E-16 ) ) ;
#8722 = AXIS2_PLACEMENT_3D ( 'NONE', #18583, #11465, #9381 ) ;
#8723 = CARTESIAN_POINT ( 'NONE',  ( 17.57831567727900079, -9.462949834988593878, 0.9681625741885133696 ) ) ;
#8724 = AXIS2_PLACEMENT_3D ( 'NONE', #15352, #22826, #21093 ) ;
#8725 = LINE ( 'NONE', #6913, #18851 ) ;
#8726 = CIRCLE ( 'NONE', #10669, 6.050000000006050982 ) ;
#8727 = LINE ( 'NONE', #7261, #23908 ) ;
#8728 = CIRCLE ( 'NONE', #22383, 1.500000000000001332 ) ;
#8729 = VERTEX_POINT ( 'NONE', #15071 ) ;
#8730 = CARTESIAN_POINT ( 'NONE',  ( -41.99999999999999289, 1.286185300804507526E-15, -10.50249999999999950 ) ) ;
#8731 = EDGE_CURVE ( 'NONE', #379, #1993, #11012, .T. ) ;
#8732 = ORIENTED_EDGE ( 'NONE', *, *, #20306, .T. ) ;
#8733 = AXIS2_PLACEMENT_3D ( 'NONE', #16077, #23047, #12165 ) ;
#8734 = CARTESIAN_POINT ( 'NONE',  ( 8.680847955711199049, -2.820578480813074496, 4.533165578109188409 ) ) ;
#8735 = DIRECTION ( 'NONE',  ( 1.000000000000000000, 0.000000000000000000, 0.000000000000000000 ) ) ;
#8736 = EDGE_CURVE ( 'NONE', #18312, #23135, #18390, .T. ) ;
#8737 = DIRECTION ( 'NONE',  ( -1.000000000000000000, -1.224606353822377258E-16, -0.000000000000000000 ) ) ;
#8738 = ORIENTED_EDGE ( 'NONE', *, *, #10397, .F. ) ;
#8739 = EDGE_CURVE ( 'NONE', #13946, #1091, #20834, .T. ) ;
#8740 = CARTESIAN_POINT ( 'NONE',  ( 71.09090909090909349, 7.491529369508391930E-15, 0.000000000000000000 ) ) ;
#8741 = CARTESIAN_POINT ( 'NONE',  ( 9.499999999999790390, 3.086737114213260025, -6.159589141758145203 ) ) ;
#8742 = EDGE_CURVE ( 'NONE', #14068, #9192, #5460, .T. ) ;
#8743 = ADVANCED_FACE ( 'NONE', ( #11532 ), #22295, .F. ) ;
#8744 = AXIS2_PLACEMENT_3D ( 'NONE', #7995, #2276, #20952 ) ;
#8745 = VECTOR ( 'NONE', #20669, 999.9999999999998863 ) ;
#8746 = DIRECTION ( 'NONE',  ( 0.000000000000000000, -1.000000000000000000, 0.000000000000000000 ) ) ;
#8747 = DIRECTION ( 'NONE',  ( 0.000000000000000000, 1.000000000000000000, -0.000000000000000000 ) ) ;
#8748 = DIRECTION ( 'NONE',  ( -0.000000000000000000, -0.000000000000000000, -1.000000000000000000 ) ) ;
#8749 = VECTOR ( 'NONE', #9834, 1000.000000000000114 ) ;
#8750 = DIRECTION ( 'NONE',  ( 1.000000000000000000, 0.000000000000000000, 0.000000000000000000 ) ) ;
#8751 = ORIENTED_EDGE ( 'NONE', *, *, #4125, .T. ) ;
#8752 = DIRECTION ( 'NONE',  ( -0.000000000000000000, -0.000000000000000000, 1.000000000000000000 ) ) ;
#8753 = CONICAL_SURFACE ( 'NONE', #6018, 1.999999999999994449, 1.029744258676653201 ) ;
#8754 = DIRECTION ( 'NONE',  ( -0.000000000000000000, -0.000000000000000000, -1.000000000000000000 ) ) ;
#8755 = ORIENTED_EDGE ( 'NONE', *, *, #1629, .T. ) ;
#8756 = DIRECTION ( 'NONE',  ( -0.000000000000000000, -0.000000000000000000, -1.000000000000000000 ) ) ;
#8757 = LINE ( 'NONE', #17805, #1281 ) ;
#8758 = CIRCLE ( 'NONE', #12269, 5.999999999999998224 ) ;
#8759 = CARTESIAN_POINT ( 'NONE',  ( 85.05659179472598908, 7.420530141404717394E-15, 0.000000000000000000 ) ) ;
#8760 = VERTEX_POINT ( 'NONE', #13009 ) ;
#8761 = CARTESIAN_POINT ( 'NONE',  ( 1.016919733032271456, 45.00000000000000000, 3.000000000000002665 ) ) ;
#8762 = SHAPE_REPRESENTATION ( 'Body', ( #8005 ), #20496 ) ;
#8764 = CIRCLE ( 'NONE', #19687, 6.050000000006050982 ) ;
#8763 = DIRECTION ( 'NONE',  ( 0.000000000000000000, 0.000000000000000000, 1.000000000000000000 ) ) ;
#8765 = ORIENTED_EDGE ( 'NONE', *, *, #15696, .T. ) ;
#8766 = VECTOR ( 'NONE', #23110, 1000.000000000000000 ) ;
#8767 = ORIENTED_EDGE ( 'NONE', *, *, #1998, .T. ) ;
#8768 = CARTESIAN_POINT ( 'NONE',  ( -5.871322893123450015, -8.081182679344781405, 12.50674201446023481 ) ) ;
#8769 = CARTESIAN_POINT ( 'NONE',  ( -7.685661446561619314, -5.583959896779019161, 8.406742014460233392 ) ) ;
#8770 = AXIS2_PLACEMENT_3D ( 'NONE', #5791, #14804, #9415 ) ;
#8771 = VERTEX_POINT ( 'NONE', #3622 ) ;
#8772 = AXIS2_PLACEMENT_3D ( 'NONE', #14976, #3418, #9251 ) ;
#8773 = DIRECTION ( 'NONE',  ( -1.000000000000000000, -1.224606353822377258E-16, -0.000000000000000000 ) ) ;
#8774 = DIRECTION ( 'NONE',  ( 0.5735764363510427177, -0.8191520442889941300, 1.003171929053527705E-16 ) ) ;
#8775 = CARTESIAN_POINT ( 'NONE',  ( 85.63636363636365445, 7.491529369508391930E-15, 0.000000000000000000 ) ) ;
#8776 = ADVANCED_FACE ( 'NONE', ( #5931 ), #22427, .T. ) ;
#8778 = EDGE_CURVE ( 'NONE', #8913, #1617, #4022, .T. ) ;
#8777 = CIRCLE ( 'NONE', #18540, 6.050000000006052758 ) ;
#8779 = FACE_OUTER_BOUND ( 'NONE', #19740, .T. ) ;
#8780 = DIRECTION ( 'NONE',  ( 0.4828336235133043330, -0.8757121056631641531, 0.000000000000000000 ) ) ;
#8781 = CARTESIAN_POINT ( 'NONE',  ( 23.90000000000000568, 29.50000000000000000, 27.00000000000000000 ) ) ;
#8782 = VERTEX_POINT ( 'NONE', #3753 ) ;
#8783 = EDGE_LOOP ( 'NONE', ( #9081, #8957, #6278, #6610 ) ) ;
#8784 =( NAMED_UNIT ( * ) SI_UNIT ( $, .STERADIAN. ) SOLID_ANGLE_UNIT ( ) );
#8785 = CARTESIAN_POINT ( 'NONE',  ( 78.94340820527399671, 7.562528597612068045E-15, 0.000000000000000000 ) ) ;
#8786 = CARTESIAN_POINT ( 'NONE',  ( 20.85000000000000853, 15.03999999999999915, 27.00000000000000000 ) ) ;
#8787 = DIRECTION ( 'NONE',  ( -1.000000000000000000, -0.000000000000000000, -0.000000000000000000 ) ) ;
#8788 = FACE_OUTER_BOUND ( 'NONE', #6612, .T. ) ;
#8789 = EDGE_CURVE ( 'NONE', #12980, #7728, #21160, .T. ) ;
#8790 = DIRECTION ( 'NONE',  ( 1.000000000000000000, 0.000000000000000000, 0.000000000000000000 ) ) ;
#8791 = CIRCLE ( 'NONE', #4135, 2.000000000000000000 ) ;
#8792 = ORIENTED_EDGE ( 'NONE', *, *, #6798, .F. ) ;
#8793 = FACE_OUTER_BOUND ( 'NONE', #18505, .T. ) ;
#8794 = ORIENTED_EDGE ( 'NONE', *, *, #12758, .F. ) ;
#8795 = ADVANCED_FACE ( 'NONE', ( #2275 ), #20342, .T. ) ;
#8796 = CARTESIAN_POINT ( 'NONE',  ( -28.27483331787887266, 41.23752903419610760, -27.00000000000000000 ) ) ;
#8797 = ORIENTED_EDGE ( 'NONE', *, *, #6470, .F. ) ;
#8798 = CARTESIAN_POINT ( 'NONE',  ( 8.417661073264035565, -2.391602252564381192, -12.49999999999999822 ) ) ;
#8799 = CARTESIAN_POINT ( 'NONE',  ( -9.500000000000211386, 3.086737114211961064, -2.959589141758143249 ) ) ;
#8800 = EDGE_CURVE ( 'NONE', #19379, #8820, #24008, .T. ) ;
#8801 = DIRECTION ( 'NONE',  ( 1.000000000000000000, 0.000000000000000000, 0.000000000000000000 ) ) ;
#8802 = VECTOR ( 'NONE', #12703, 1000.000000000000000 ) ;
#8803 = AXIS2_PLACEMENT_3D ( 'NONE', #10361, #14740, #10933 ) ;
#8804 = CARTESIAN_POINT ( 'NONE',  ( 41.00000000000000000, -26.23076770084981391, 12.00000000000000000 ) ) ;
#8805 = CYLINDRICAL_SURFACE ( 'NONE', #6123, 14.72592346043842326 ) ;
#8806 = AXIS2_PLACEMENT_3D ( 'NONE', #16389, #1767, #9193 ) ;
#8807 = CONICAL_SURFACE ( 'NONE', #5722, 4.172000000000008590, 0.9599310885968742602 ) ;
#8808 = CARTESIAN_POINT ( 'NONE',  ( -9.500000000000000000, -6.482511860946779655E-13, -4.206742014460233214 ) ) ;
#8809 = ORIENTED_EDGE ( 'NONE', *, *, #13320, .F. ) ;
#8810 = ORIENTED_EDGE ( 'NONE', *, *, #7533, .T. ) ;
#8811 = DIRECTION ( 'NONE',  ( -0.000000000000000000, -0.000000000000000000, 1.000000000000000000 ) ) ;
#8812 = DIRECTION ( 'NONE',  ( -1.000000000000000000, 0.000000000000000000, 0.000000000000000000 ) ) ;
#8813 = CARTESIAN_POINT ( 'NONE',  ( 40.99749999999998096, 5.618459588085056979E-15, 0.000000000000000000 ) ) ;
#8814 = ORIENTED_EDGE ( 'NONE', *, *, #12440, .T. ) ;
#8815 = VECTOR ( 'NONE', #3137, 1000.000000000000000 ) ;
#8816 = CARTESIAN_POINT ( 'NONE',  ( 7.685661446562381371, -5.583959896777971110, -3.859589141758143604 ) ) ;
#8817 = AXIS2_PLACEMENT_3D ( 'NONE', #951, #10189, #23291 ) ;
#8818 = AXIS2_PLACEMENT_3D ( 'NONE', #6999, #18124, #21538 ) ;
#8819 = DIRECTION ( 'NONE',  ( -0.5735764363510519326, 0.8191520442889876907, 1.003171929053519816E-16 ) ) ;
#8820 = VERTEX_POINT ( 'NONE', #4235 ) ;
#8821 = CARTESIAN_POINT ( 'NONE',  ( -40.66734255040738333, 26.56420859267091927, -3.000000000000000000 ) ) ;
#8822 = EDGE_CURVE ( 'NONE', #12778, #17472, #21318, .T. ) ;
#8823 = DIRECTION ( 'NONE',  ( 0.000000000000000000, 0.000000000000000000, -1.000000000000000000 ) ) ;
#8824 = LINE ( 'NONE', #20060, #8010 ) ;
#8825 = TOROIDAL_SURFACE ( 'NONE', #20920, 10.49999999999999822, 1.000000000000000000 ) ;
#8826 = LINE ( 'NONE', #3100, #1232 ) ;
#8827 = ORIENTED_EDGE ( 'NONE', *, *, #1981, .F. ) ;
#8828 = ORIENTED_EDGE ( 'NONE', *, *, #8016, .T. ) ;
#8829 = EDGE_LOOP ( 'NONE', ( #11520, #1999, #22604, #21133 ) ) ;
#8830 = ORIENTED_EDGE ( 'NONE', *, *, #22568, .T. ) ;
#8831 = DIRECTION ( 'NONE',  ( -1.000000000000000000, 0.000000000000000000, 0.000000000000000000 ) ) ;
#8832 = CONICAL_SURFACE ( 'NONE', #661, 9.499999999999996447, 0.7853981633974482790 ) ;
#8833 =( NAMED_UNIT ( * ) SI_UNIT ( $, .STERADIAN. ) SOLID_ANGLE_UNIT ( ) );
#8834 = CARTESIAN_POINT ( 'NONE',  ( 5.000000000000000000, 0.000000000000000000, 0.000000000000000000 ) ) ;
#8835 = DIRECTION ( 'NONE',  ( -0.000000000000000000, -0.000000000000000000, 1.000000000000000000 ) ) ;
#8836 = VERTEX_POINT ( 'NONE', #4355 ) ;
#8837 = VERTEX_POINT ( 'NONE', #11762 ) ;
#8838 = CARTESIAN_POINT ( 'NONE',  ( 77.48886275072855767, -5.000000000000000888, 6.123233995736776143E-16 ) ) ;
#8839 = ORIENTED_EDGE ( 'NONE', *, *, #2341, .F. ) ;
#8840 = DIRECTION ( 'NONE',  ( 0.7052211081716915908, -0.7089874389501490404, 0.000000000000000000 ) ) ;
#8841 = CARTESIAN_POINT ( 'NONE',  ( 0.000000000000000000, 0.000000000000000000, 27.00000000000000000 ) ) ;
#8842 = CARTESIAN_POINT ( 'NONE',  ( 5.871322893124553133, -8.081182679343980269, 6.906742014460234280 ) ) ;
#8843 = FACE_OUTER_BOUND ( 'NONE', #18026, .T. ) ;
#8844 = DIRECTION ( 'NONE',  ( -1.000000000000000000, -1.224606353822377258E-16, -0.000000000000000000 ) ) ;
#8845 = EDGE_CURVE ( 'NONE', #6675, #3315, #14331, .T. ) ;
#8846 = CARTESIAN_POINT ( 'NONE',  ( 23.85000000000000497, 15.03999999999999915, -25.00000000000000000 ) ) ;
#8847 = ADVANCED_FACE ( 'NONE', ( #22038 ), #14488, .T. ) ;
#8848 = CARTESIAN_POINT ( 'NONE',  ( -7.022953521754877748, -5.102474405760673015, -3.833165578109188676 ) ) ;
#8849 = EDGE_CURVE ( 'NONE', #12921, #3740, #9788, .T. ) ;
#8850 = DIRECTION ( 'NONE',  ( 0.000000000000000000, 0.000000000000000000, 1.000000000000000000 ) ) ;
#8851 = VERTEX_POINT ( 'NONE', #23747 ) ;
#8852 = CARTESIAN_POINT ( 'NONE',  ( -7.022953521755574080, 5.102474405759713783, 11.43316557810918965 ) ) ;
#8853 = EDGE_LOOP ( 'NONE', ( #14283, #9883, #17843, #14807 ) ) ;
#8854 = PRODUCT_DEFINITION_SHAPE ( 'NONE', 'NONE',  #10008 ) ;
#8855 = APPLICATION_PROTOCOL_DEFINITION ( 'draft international standard', 'automotive_design', 1998, #3548 ) ;
#8856 = PLANE ( 'NONE',  #21039 ) ;
#8857 = VERTEX_POINT ( 'NONE', #10433 ) ;
#8858 = ORIENTED_EDGE ( 'NONE', *, *, #13630, .T. ) ;
#8859 = CARTESIAN_POINT ( 'NONE',  ( 35.99999999999999289, 50.99999999999999289, 0.000000000000000000 ) ) ;
#8860 = CARTESIAN_POINT ( 'NONE',  ( -6.822232771736903637E-13, 9.988891130263535700, -6.559589141758143782 ) ) ;
#8861 = CARTESIAN_POINT ( 'NONE',  ( -2.258808436415836507, 8.713077898639953744, 100.9837996669589728 ) ) ;
#8862 = DIRECTION ( 'NONE',  ( -1.000000000000000000, -0.000000000000000000, -0.000000000000000000 ) ) ;
#8863 = CARTESIAN_POINT ( 'NONE',  ( 20.85000000000000853, 15.03999999999999915, -25.00000000000000000 ) ) ;
#8864 = CARTESIAN_POINT ( 'NONE',  ( -29.00000000000000000, 29.49999999999999645, 11.00000000000000000 ) ) ;
#8865 = CARTESIAN_POINT ( 'NONE',  ( 0.000000000000000000, 0.000000000000000000, 9.000000000000000000 ) ) ;
#8866 = EDGE_CURVE ( 'NONE', #23300, #19009, #7130, .T. ) ;
#8867 = VERTEX_POINT ( 'NONE', #17894 ) ;
#8868 = CARTESIAN_POINT ( 'NONE',  ( 29.00000000000000000, 29.50000000000000000, -3.000000000000000000 ) ) ;
#8869 = ORIENTED_EDGE ( 'NONE', *, *, #17076, .T. ) ;
#8870 = DIRECTION ( 'NONE',  ( -6.938893903907221278E-15, 1.000000000000000000, 6.938893903907221278E-15 ) ) ;
#8871 = CARTESIAN_POINT ( 'NONE',  ( 41.73082370883257397, -27.62204025492843940, -3.000000000000000000 ) ) ;
#8872 = CARTESIAN_POINT ( 'NONE',  ( 17.49232137458055192, 9.205685982891283814, -2.395442301836272936 ) ) ;
#8873 = EDGE_CURVE ( 'NONE', #10011, #14307, #14568, .T. ) ;
#8874 = CARTESIAN_POINT ( 'NONE',  ( -30.00000000000000355, -3.851859888774471706E-31, 10.49999999999999822 ) ) ;
#8875 = EDGE_CURVE ( 'NONE', #831, #13710, #18407, .T. ) ;
#8876 = VERTEX_POINT ( 'NONE', #19441 ) ;
#8877 = DIRECTION ( 'NONE',  ( 0.000000000000000000, 1.000000000000000000, -1.224646799147353207E-16 ) ) ;
#8878 = CARTESIAN_POINT ( 'NONE',  ( 9.500000000000000000, 6.470877716354879437E-13, -9.206742014460234103 ) ) ;
#8879 = EDGE_CURVE ( 'NONE', #4920, #19859, #4569, .T. ) ;
#8880 = ADVANCED_FACE ( 'NONE', ( #19189 ), #13749, .F. ) ;
#8881 = CYLINDRICAL_SURFACE ( 'NONE', #23797, 1.500000000000001332 ) ;
#8882 = ORIENTED_EDGE ( 'NONE', *, *, #19095, .T. ) ;
#8883 = EDGE_LOOP ( 'NONE', ( #11410, #21849, #13951, #22480 ) ) ;
#8884 = CARTESIAN_POINT ( 'NONE',  ( -9.499999999999790390, -3.086737114213257804, 10.30674201446023375 ) ) ;
#8885 = CARTESIAN_POINT ( 'NONE',  ( 2.935661446562616295, -9.035036904803758873, 6.806742014460233747 ) ) ;
#8886 = CARTESIAN_POINT ( 'NONE',  ( 67.30704456891035647, 7.562528597612068045E-15, 0.000000000000000000 ) ) ;
#8887 = AXIS2_PLACEMENT_3D ( 'NONE', #15063, #16769, #14820 ) ;
#8888 = ORIENTED_EDGE ( 'NONE', *, *, #7793, .F. ) ;
#8889 =( NAMED_UNIT ( * ) PLANE_ANGLE_UNIT ( ) SI_UNIT ( $, .RADIAN. ) );
#8890 = DIRECTION ( 'NONE',  ( 0.000000000000000000, 0.000000000000000000, -1.000000000000000000 ) ) ;
#8891 = FACE_OUTER_BOUND ( 'NONE', #19921, .T. ) ;
#8892 = DIRECTION ( 'NONE',  ( -0.000000000000000000, -0.000000000000000000, -1.000000000000000000 ) ) ;
#8893 = EDGE_CURVE ( 'NONE', #3007, #21144, #12926, .T. ) ;
#8894 = LINE ( 'NONE', #5732, #16177 ) ;
#8895 = CYLINDRICAL_SURFACE ( 'NONE', #2395, 1.499999999999994449 ) ;
#8896 = DIRECTION ( 'NONE',  ( -1.000000000000000000, -1.224606353822377258E-16, -0.000000000000000000 ) ) ;
#8897 = CARTESIAN_POINT ( 'NONE',  ( 88.54545454545454675, 7.491529369508391930E-15, 0.000000000000000000 ) ) ;
#8898 = VECTOR ( 'NONE', #19297, 1000.000000000000000 ) ;
#8899 =( BOUNDED_CURVE ( )  B_SPLINE_CURVE ( 2, ( #6862, #20271, #18088, #12450, #1381, #20038, #3670, #8799, #23809, #14764, #1500, #16246, #22122 ),
 .UNSPECIFIED., .F., .T. ) 
 B_SPLINE_CURVE_WITH_KNOTS ( ( 3, 2, 2, 2, 2, 2, 3 ),
 ( 0.8558632199373886751, 0.8599999999999999867, 0.8800000000000000044, 0.9000000000000000222, 0.9200000000000000400, 0.9399999999999999467, 0.9500000000000000666 ),
 .UNSPECIFIED. ) 
 CURVE ( )  GEOMETRIC_REPRESENTATION_ITEM ( )  RATIONAL_B_SPLINE_CURVE ( ( 0.9839409940142134214, 0.9898765786207525119, 1.000000000000000000, 0.9510565162951535312, 1.000000000000000000, 0.9510565162951535312, 1.000000000000000000, 0.9510565162951535312, 1.000000000000000000, 0.9510565162951535312, 1.000000000000000000, 0.9755282581475764880, 0.9755282581475768211 ) ) 
 REPRESENTATION_ITEM ( '' )  );
#8900 = CARTESIAN_POINT ( 'NONE',  ( 0.000000000000000000, 3.378881074890309311, 11.18737882312122878 ) ) ;
#8901 = EDGE_CURVE ( 'NONE', #21063, #1690, #20739, .T. ) ;
#8902 = DIRECTION ( 'NONE',  ( -1.000000000000000000, 0.000000000000000000, 0.000000000000000000 ) ) ;
#8903 = EDGE_LOOP ( 'NONE', ( #4996, #11895, #15586, #8984 ) ) ;
#8904 = CARTESIAN_POINT ( 'NONE',  ( 9.499999999999799272, 3.086737114213245370, -6.159589141758142539 ) ) ;
#8905 = ORIENTED_EDGE ( 'NONE', *, *, #23866, .F. ) ;
#8906 = DIRECTION ( 'NONE',  ( -1.000000000000000000, 0.000000000000000000, 0.000000000000000000 ) ) ;
#8907 = FACE_OUTER_BOUND ( 'NONE', #15635, .T. ) ;
#8908 = CLOSED_SHELL ( 'NONE', ( #12140, #6015, #18998, #4175, #11538, #1127, #11921, #24028, #23383, #21479, #10214, #1552, #1511, #6212, #11714, #21229, #2555, #13446, #6347, #18062, #13467, #740, #4258, #6997, #4424, #21339, #15494, #1585, #16474, #4887, #2714, #13057, #12132, #20978, #1382, #13160, #21166, #18441, #23139, #17759, #10249, #2879, #10498, #23972, #18253, #1187, #11103, #6131, #10887, #1258, #8342, #9002, #22290, #7893, #23812, #21553, #5045, #5108, #9275, #9166, #7645, #18819, #8136, #14971, #3268, #19636, #11213, #19704, #14631, #16941, #8567, #15954, #18589, #508, #19877, #22517, #16408, #12648, #7506, #7751, #1435, #15633, #8543, #8192, #20926, #16943, #12104, #3537, #18280, #12138, #16914, #2009, #19860, #14765, #1071, #12235, #2556, #6707, #5339, #18115, #22935, #12032, #17025, #656, #21776, #20954, #23714, #5775, #19125, #571, #19787, #2187, #23032, #10065, #17493, #2316, #6738, #19243, #12351, #18709, #2240, #12052, #19754, #23787, #23435, #11029, #17046, #18684, #6415, #20900, #15064, #4096, #6960, #10888, #14786 ) ) ;
#8909 = ORIENTED_EDGE ( 'NONE', *, *, #17360, .T. ) ;
#8910 = CARTESIAN_POINT ( 'NONE',  ( 40.77574956473004164, -27.49633847812775755, 0.000000000000000000 ) ) ;
#8911 = DIRECTION ( 'NONE',  ( -0.000000000000000000, -0.000000000000000000, 1.000000000000000000 ) ) ;
#8912 = LINE ( 'NONE', #11085, #20105 ) ;
#8913 = VERTEX_POINT ( 'NONE', #13663 ) ;
#8914 = LINE ( 'NONE', #7087, #13355 ) ;
#8915 = FACE_OUTER_BOUND ( 'NONE', #9868, .T. ) ;
#8916 = CARTESIAN_POINT ( 'NONE',  ( 2.935661446561383503, 9.035036904804158553, -7.606742014460233570 ) ) ;
#8917 = ORIENTED_EDGE ( 'NONE', *, *, #21348, .T. ) ;
#8918 = DIRECTION ( 'NONE',  ( -1.000000000000000000, -1.224606353822377258E-16, -0.000000000000000000 ) ) ;
#8919 = EDGE_CURVE ( 'NONE', #8263, #4207, #12537, .T. ) ;
#8920 = TOROIDAL_SURFACE ( 'NONE', #12028, 3.500000000000001776, 1.500000000000000000 ) ;
#8921 = CARTESIAN_POINT ( 'NONE',  ( -36.00000000000001421, 50.99999999999999289, 0.5000000000000000000 ) ) ;
#8922 = CARTESIAN_POINT ( 'NONE',  ( -41.50000000000000000, 28.80990663662250739, 11.00000000000000000 ) ) ;
#8923 = ORIENTED_EDGE ( 'NONE', *, *, #18999, .F. ) ;
#8924 = EDGE_CURVE ( 'NONE', #22742, #22311, #8283, .T. ) ;
#8925 = CARTESIAN_POINT ( 'NONE',  ( -7.561939491010504000, 5.750397476200735269, 11.99999999999999822 ) ) ;
#8926 = LINE ( 'NONE', #11104, #7521 ) ;
#8927 = EDGE_LOOP ( 'NONE', ( #14774, #1877, #16315, #690, #15278 ) ) ;
#8928 = CARTESIAN_POINT ( 'NONE',  ( -34.00000000000000000, -5.999999999999999112, 11.00000000000000000 ) ) ;
#8929 = AXIS2_PLACEMENT_3D ( 'NONE', #14090, #8216, #17398 ) ;
#8930 = CARTESIAN_POINT ( 'NONE',  ( 86.21613547800127719, -1.078520768856852078E-29, 5.000000000000007994 ) ) ;
#8931 = PLANE ( 'NONE',  #2566 ) ;
#8932 = DIRECTION ( 'NONE',  ( -0.7071067811865487940, 8.659560562354948882E-17, 0.7071067811865463515 ) ) ;
#8933 = ORIENTED_EDGE ( 'NONE', *, *, #10122, .T. ) ;
#8934 = AXIS2_PLACEMENT_3D ( 'NONE', #12277, #23406, #19748 ) ;
#8935 = ORIENTED_EDGE ( 'NONE', *, *, #4431, .F. ) ;
#8936 = ORIENTED_EDGE ( 'NONE', *, *, #17660, .F. ) ;
#8937 = CARTESIAN_POINT ( 'NONE',  ( -41.00000000000000000, -5.000000000000000888, 9.500000000000000000 ) ) ;
#8938 = EDGE_CURVE ( 'NONE', #192, #21201, #9735, .T. ) ;
#8939 = CARTESIAN_POINT ( 'NONE',  ( 1.255262969126036846E-16, -14.99147757894464306, 8.775000000000000355 ) ) ;
#8940 = ORIENTED_EDGE ( 'NONE', *, *, #1914, .T. ) ;
#8941 = ORIENTED_EDGE ( 'NONE', *, *, #16550, .T. ) ;
#8942 = CARTESIAN_POINT ( 'NONE',  ( -14.80736872429922002, -4.130115634539735403, -8.564444421911375116 ) ) ;
#8943 = ADVANCED_FACE ( 'NONE', ( #7914, #19414, #22836, #2207, #2691, #10105, #17078, #378 ), #6223, .F. ) ;
#8944 = CARTESIAN_POINT ( 'NONE',  ( 1.999999999999994449, 45.00000000000000000, -27.00000000000000000 ) ) ;
#8945 = ORIENTED_EDGE ( 'NONE', *, *, #17424, .F. ) ;
#8946 = CYLINDRICAL_SURFACE ( 'NONE', #8806, 1.000000000000002442 ) ;
#8947 = CARTESIAN_POINT ( 'NONE',  ( 90.00000000000000000, 0.000000000000000000, 4.171999999999999709 ) ) ;
#8948 = CARTESIAN_POINT ( 'NONE',  ( -9.500000000000202505, 3.086737114211975275, 6.106742014460232681 ) ) ;
#8949 = DIRECTION ( 'NONE',  ( 0.000000000000000000, 0.000000000000000000, 1.000000000000000000 ) ) ;
#8950 = DIRECTION ( 'NONE',  ( 1.000000000000000000, 0.000000000000000000, 0.000000000000000000 ) ) ;
#8951 = DIRECTION ( 'NONE',  ( -0.5735764363510517105, -0.8191520442889879128, 0.000000000000000000 ) ) ;
#8952 = CIRCLE ( 'NONE', #19499, 8.999999999999998224 ) ;
#8953 = LINE ( 'NONE', #23749, #5996 ) ;
#8954 = CARTESIAN_POINT ( 'NONE',  ( -8.680847955711200825, 2.820578480813073607, -3.533165578109187965 ) ) ;
#8955 = DIRECTION ( 'NONE',  ( -1.000000000000000000, -0.000000000000000000, 0.000000000000000000 ) ) ;
#8956 = CARTESIAN_POINT ( 'NONE',  ( -8.680847955711007202, -5.923547351154968927E-13, 11.63316557810919072 ) ) ;
#8957 = ORIENTED_EDGE ( 'NONE', *, *, #8322, .T. ) ;
#8958 = CARTESIAN_POINT ( 'NONE',  ( 693.7818939062881327, 888.4837211537981148, 1347.481724745927977 ) ) ;
#8959 = CARTESIAN_POINT ( 'NONE',  ( 41.99999999999999289, 25.93535998569253920, 27.00000000000000000 ) ) ;
#8960 = ORIENTED_EDGE ( 'NONE', *, *, #17629, .T. ) ;
#8961 = ORIENTED_EDGE ( 'NONE', *, *, #6251, .T. ) ;
#8962 = DIRECTION ( 'NONE',  ( -0.7071067811865474617, 0.000000000000000000, -0.7071067811865474617 ) ) ;
#8963 = CARTESIAN_POINT ( 'NONE',  ( 2.935661446562616295, -9.035036904803758873, -9.659589141758143427 ) ) ;
#8964 = AXIS2_PLACEMENT_3D ( 'NONE', #6368, #11703, #16212 ) ;
#8965 = PLANE ( 'NONE',  #7163 ) ;
#8966 = DIRECTION ( 'NONE',  ( -0.000000000000000000, 0.000000000000000000, 1.000000000000000000 ) ) ;
#8967 = DIRECTION ( 'NONE',  ( 0.000000000000000000, -1.000000000000000000, 0.000000000000000000 ) ) ;
#8968 = EDGE_CURVE ( 'NONE', #23710, #16661, #2026, .T. ) ;
#8969 = EDGE_CURVE ( 'NONE', #9146, #2741, #4037, .T. ) ;
#8970 = CARTESIAN_POINT ( 'NONE',  ( 5.000000000000000000, 2.342598717236913153, 4.057500000000004547 ) ) ;
#8971 = ORIENTED_EDGE ( 'NONE', *, *, #8187, .T. ) ;
#8972 = CARTESIAN_POINT ( 'NONE',  ( 9.500000000000000000, 6.470877716354879437E-13, -7.206742014460234103 ) ) ;
#8973 = ORIENTED_EDGE ( 'NONE', *, *, #9879, .T. ) ;
#8974 = CARTESIAN_POINT ( 'NONE',  ( 15.00000000000000355, 15.50000000000000000, 7.700000000000001954 ) ) ;
#8975 = LINE ( 'NONE', #5712, #19935 ) ;
#8976 = DIRECTION ( 'NONE',  ( 1.000000000000000000, 0.000000000000000000, 0.000000000000000000 ) ) ;
#8977 = DIRECTION ( 'NONE',  ( 0.000000000000000000, 0.000000000000000000, -1.000000000000000000 ) ) ;
#8978 = B_SPLINE_CURVE_WITH_KNOTS ( 'NONE', 3,
 ( #11644, #15178, #15551, #22649 ),
 .UNSPECIFIED., .F., .F.,
 ( 4, 4 ),
 ( 0.000000000000000000, 1.000000000000000000 ),
 .UNSPECIFIED. ) ;
#8979 = DIRECTION ( 'NONE',  ( 1.000000000000000000, 0.000000000000000000, 0.000000000000000000 ) ) ;
#8980 = ORIENTED_EDGE ( 'NONE', *, *, #7694, .F. ) ;
#8981 = DIRECTION ( 'NONE',  ( 0.000000000000000000, -1.000000000000000000, 0.000000000000000000 ) ) ;
#8982 = CARTESIAN_POINT ( 'NONE',  ( 9.500000000000000000, 6.470877716354879437E-13, -11.20674201446023410 ) ) ;
#8983 = ORIENTED_EDGE ( 'NONE', *, *, #4062, .T. ) ;
#8984 = ORIENTED_EDGE ( 'NONE', *, *, #7438, .T. ) ;
#8985 = AXIS2_PLACEMENT_3D ( 'NONE', #703, #15820, #19616 ) ;
#8986 = CARTESIAN_POINT ( 'NONE',  ( -5.871322893123450015, -8.081182679344781405, 8.506742014460233037 ) ) ;
#8987 = CARTESIAN_POINT ( 'NONE',  ( -9.499999999999790390, -3.086737114213257804, 8.306742014460233747 ) ) ;
#8988 = EDGE_LOOP ( 'NONE', ( #22751, #18238, #2894 ) ) ;
#8989 = PRODUCT_DEFINITION ( 'UNKNOWN', '', #13904, #7959 ) ;
#8990 = VECTOR ( 'NONE', #8721, 1000.000000000000000 ) ;
#8991 = VERTEX_POINT ( 'NONE', #20994 ) ;
#8992 = CARTESIAN_POINT ( 'NONE',  ( 0.000000000000000000, 0.000000000000000000, 0.000000000000000000 ) ) ;
#8993 = ADVANCED_FACE ( 'NONE', ( #17447 ), #8250, .T. ) ;
#8994 = PLANE ( 'NONE',  #10228 ) ;
#8995 = DIRECTION ( 'NONE',  ( 0.000000000000000000, -1.000000000000000000, 0.000000000000000000 ) ) ;
#8996 = CARTESIAN_POINT ( 'NONE',  ( -40.00000000000000000, 0.000000000000000000, 0.000000000000000000 ) ) ;
#8997 = ADVANCED_FACE ( 'NONE', ( #15225 ), #15869, .T. ) ;
#8998 = ADVANCED_BREP_SHAPE_REPRESENTATION ( '', ( #2111, #8005 ), #2575 ) ;
#8999 = CARTESIAN_POINT ( 'NONE',  ( 41.00000000000000000, 0.000000000000000000, 11.00000000000000000 ) ) ;
#9000 = FACE_OUTER_BOUND ( 'NONE', #413, .T. ) ;
#9001 = CARTESIAN_POINT ( 'NONE',  ( 40.29291594121673370, 26.62062637246459218, 12.00000000000000000 ) ) ;
#9002 = ADVANCED_FACE ( 'NONE', ( #23329 ), #21730, .F. ) ;
#9003 = EDGE_CURVE ( 'NONE', #16254, #1315, #23855, .T. ) ;
#9004 = ORIENTED_EDGE ( 'NONE', *, *, #12912, .T. ) ;
#9005 = VECTOR ( 'NONE', #1486, 1000.000000000000000 ) ;
#9006 = AXIS2_PLACEMENT_3D ( 'NONE', #13727, #13865, #18863 ) ;
#9007 = ORIENTED_EDGE ( 'NONE', *, *, #21131, .F. ) ;
#9008 = FACE_OUTER_BOUND ( 'NONE', #14049, .T. ) ;
#9009 = CIRCLE ( 'NONE', #22659, 5.000000000000007994 ) ;
#9010 = CARTESIAN_POINT ( 'NONE',  ( 0.000000000000000000, -45.00000000000000000, -3.000000000000000000 ) ) ;
#9011 = CARTESIAN_POINT ( 'NONE',  ( -9.500000000000000000, -6.482511860946779655E-13, -11.05958914175814556 ) ) ;
#9012 = CARTESIAN_POINT ( 'NONE',  ( 23.00000000000000000, -13.66196005206961850, -3.918670437617226110 ) ) ;
#9013 = LINE ( 'NONE', #3427, #19305 ) ;
#9014 = EDGE_LOOP ( 'NONE', ( #22353, #20462, #14598, #12246 ) ) ;
#9015 = FACE_OUTER_BOUND ( 'NONE', #13139, .T. ) ;
#9016 = EDGE_LOOP ( 'NONE', ( #3041, #2493 ) ) ;
#9017 = CARTESIAN_POINT ( 'NONE',  ( 67.60204634018053582, -9.244463733058732095E-30, 5.000000000000007994 ) ) ;
#9018 = ORIENTED_EDGE ( 'NONE', *, *, #10913, .F. ) ;
#9019 = DIRECTION ( 'NONE',  ( -1.000000000000000000, 0.000000000000000000, 0.000000000000000000 ) ) ;
#9020 = DIRECTION ( 'NONE',  ( 0.000000000000000000, -1.000000000000000000, 0.000000000000000000 ) ) ;
#9021 = EDGE_CURVE ( 'NONE', #6097, #18287, #6716, .T. ) ;
#9022 = DIRECTION ( 'NONE',  ( -0.7071067811865660024, 0.000000000000000000, -0.7071067811865291430 ) ) ;
#9023 = VECTOR ( 'NONE', #2552, 1000.000000000000000 ) ;
#9024 = AXIS2_PLACEMENT_3D ( 'NONE', #1335, #3043, #12771 ) ;
#9025 = AXIS2_PLACEMENT_3D ( 'NONE', #22580, #13666, #13427 ) ;
#9026 = CARTESIAN_POINT ( 'NONE',  ( -28.99999999999999645, 29.50000000000000000, -27.00000000000000000 ) ) ;
#9027 = AXIS2_PLACEMENT_3D ( 'NONE', #5858, #18926, #13422 ) ;
#9028 = ORIENTED_EDGE ( 'NONE', *, *, #9077, .F. ) ;
#9029 = CYLINDRICAL_SURFACE ( 'NONE', #12188, 11.00000000000000711 ) ;
#9030 = EDGE_CURVE ( 'NONE', #20616, #12416, #10970, .T. ) ;
#9031 = CARTESIAN_POINT ( 'NONE',  ( -28.99999999999998579, -29.50000000000000711, -3.000000000000000000 ) ) ;
#9032 = ADVANCED_FACE ( 'NONE', ( #1483 ), #2822, .T. ) ;
#9033 = CARTESIAN_POINT ( 'NONE',  ( 9.500000000000209610, -3.086737114211962396, -9.959589141758145914 ) ) ;
#9034 = ORIENTED_EDGE ( 'NONE', *, *, #11087, .T. ) ;
#9035 = ORIENTED_EDGE ( 'NONE', *, *, #7159, .F. ) ;
#9036 = CARTESIAN_POINT ( 'NONE',  ( 61.78386452199871570, -9.244463733058732095E-30, 5.000000000000007994 ) ) ;
#9037 = DIRECTION ( 'NONE',  ( -1.000000000000000000, 0.000000000000000000, 0.000000000000000000 ) ) ;
#9038 = PLANE ( 'NONE',  #731 ) ;
#9039 = CIRCLE ( 'NONE', #22688, 2.024999999999999911 ) ;
#9040 = VECTOR ( 'NONE', #8308, 1000.000000000000227 ) ;
#9041 = EDGE_LOOP ( 'NONE', ( #15872, #22085 ) ) ;
#9042 = AXIS2_PLACEMENT_3D ( 'NONE', #17304, #2417, #15710 ) ;
#9043 = CARTESIAN_POINT ( 'NONE',  ( 29.00000000000000000, 29.50000000000000355, 12.00000000000000000 ) ) ;
#9044 = CIRCLE ( 'NONE', #15660, 4.172000000000008590 ) ;
#9045 = CARTESIAN_POINT ( 'NONE',  ( 14.98950073861089294, -0.6491375924673296050, 9.483449329262333194 ) ) ;
#9046 = AXIS2_PLACEMENT_3D ( 'NONE', #9550, #3587, #24086 ) ;
#9047 = CARTESIAN_POINT ( 'NONE',  ( 0.000000000000000000, 0.000000000000000000, -3.499999999999999556 ) ) ;
#9048 = ORIENTED_EDGE ( 'NONE', *, *, #1359, .T. ) ;
#9049 = AXIS2_PLACEMENT_3D ( 'NONE', #3562, #1747, #36 ) ;
#9050 = DIRECTION ( 'NONE',  ( -1.000000000000000000, 0.000000000000000000, 0.000000000000000000 ) ) ;
#9051 = CARTESIAN_POINT ( 'NONE',  ( 40.49999999999998579, -51.00000000000000711, 0.5000000000000004441 ) ) ;
#9052 = CARTESIAN_POINT ( 'NONE',  ( -6.153822176767817416E-13, 9.500000000000000000, -3.706742014460231882 ) ) ;
#9053 = CARTESIAN_POINT ( 'NONE',  ( -9.500000000000000000, -6.482511860946779655E-13, 3.059589141758143338 ) ) ;
#9054 = EDGE_LOOP ( 'NONE', ( #13822, #20218, #18917, #6253 ) ) ;
#9055 = ORIENTED_EDGE ( 'NONE', *, *, #16738, .T. ) ;
#9056 = EDGE_LOOP ( 'NONE', ( #4316, #7402, #17254, #10469 ) ) ;
#9057 = VECTOR ( 'NONE', #14944, 1000.000000000000000 ) ;
#9058 = CIRCLE ( 'NONE', #4001, 1.000000000000000888 ) ;
#9059 = LINE ( 'NONE', #5663, #12320 ) ;
#9060 = ADVANCED_FACE ( 'NONE', ( #9131 ), #14973, .F. ) ;
#9061 = VECTOR ( 'NONE', #23009, 1000.000000000000000 ) ;
#9062 = CIRCLE ( 'NONE', #18035, 5.000000000000007994 ) ;
#9063 = CIRCLE ( 'NONE', #6341, 6.050000000006050094 ) ;
#9064 = FACE_OUTER_BOUND ( 'NONE', #16367, .T. ) ;
#9065 = ORIENTED_EDGE ( 'NONE', *, *, #10905, .F. ) ;
#9066 = CIRCLE ( 'NONE', #11789, 2.024999999999999911 ) ;
#9067 = CARTESIAN_POINT ( 'NONE',  ( 73.12522638709218370, 7.562528597612068045E-15, 0.000000000000000000 ) ) ;
#9068 = AXIS2_PLACEMENT_3D ( 'NONE', #2139, #5692, #7731 ) ;
#9069 = ORIENTED_EDGE ( 'NONE', *, *, #15585, .T. ) ;
#9070 = CARTESIAN_POINT ( 'NONE',  ( 3.000000000000000888, 8.485281374238567764, 80.99999999999998579 ) ) ;
#9071 = CARTESIAN_POINT ( 'NONE',  ( -20.84999999999999787, -16.67999999999985050, 14.50000000000000000 ) ) ;
#9072 = DIRECTION ( 'NONE',  ( -0.000000000000000000, -0.000000000000000000, -1.000000000000000000 ) ) ;
#9073 = CIRCLE ( 'NONE', #13758, 2.000000000000000000 ) ;
#9074 = DIRECTION ( 'NONE',  ( -1.000000000000000000, 0.000000000000000000, 0.000000000000000000 ) ) ;
#9075 = FACE_OUTER_BOUND ( 'NONE', #17065, .T. ) ;
#9076 = VECTOR ( 'NONE', #14360, 1000.000000000000000 ) ;
#9077 = EDGE_CURVE ( 'NONE', #17802, #16134, #11741, .T. ) ;
#9078 = CARTESIAN_POINT ( 'NONE',  ( -14.91624121966758842, 1.615102390220944706, -9.367332145225624629 ) ) ;
#9079 = AXIS2_PLACEMENT_3D ( 'NONE', #9551, #13212, #2487 ) ;
#9080 = AXIS2_PLACEMENT_3D ( 'NONE', #16557, #24011, #12886 ) ;
#9081 = ORIENTED_EDGE ( 'NONE', *, *, #14208, .F. ) ;
#9082 = CARTESIAN_POINT ( 'NONE',  ( -2.682529543899159208, -8.255977015246598327, 8.033165578109189298 ) ) ;
#9083 = EDGE_LOOP ( 'NONE', ( #8601, #19186, #17744, #18090, #4256, #1986 ) ) ;
#9084 = AXIS2_PLACEMENT_3D ( 'NONE', #1620, #23952, #4823 ) ;
#9085 = EDGE_CURVE ( 'NONE', #19174, #18693, #20304, .T. ) ;
#9086 = CIRCLE ( 'NONE', #23913, 12.73082370883259884 ) ;
#9087 = APPLICATION_PROTOCOL_DEFINITION ( 'draft international standard', 'automotive_design', 1998, #6978 ) ;
#9088 = EDGE_CURVE ( 'NONE', #22311, #15590, #3527, .T. ) ;
#9089 = FACE_OUTER_BOUND ( 'NONE', #2352, .T. ) ;
#9090 = ORIENTED_EDGE ( 'NONE', *, *, #7611, .F. ) ;
#9091 = ORIENTED_EDGE ( 'NONE', *, *, #2798, .F. ) ;
#9092 = EDGE_CURVE ( 'NONE', #24045, #1813, #16798, .T. ) ;
#9093 = DIRECTION ( 'NONE',  ( -0.000000000000000000, -0.000000000000000000, -1.000000000000000000 ) ) ;
#9094 = CARTESIAN_POINT ( 'NONE',  ( -5.365059087798939252, -7.384370330707086261, -11.93316557810918965 ) ) ;
#9096 = AXIS2_PLACEMENT_3D ( 'NONE', #9995, #17451, #17562 ) ;
#9095 = CARTESIAN_POINT ( 'NONE',  ( -20.84999999999999787, 16.67999999999985405, 13.50000000000000178 ) ) ;
#9097 = VECTOR ( 'NONE', #18972, 1000.000000000000000 ) ;
#9098 = DIRECTION ( 'NONE',  ( 0.000000000000000000, 1.000000000000000000, 0.000000000000000000 ) ) ;
#9099 = VERTEX_POINT ( 'NONE', #15199 ) ;
#9100 = LINE ( 'NONE', #1910, #14883 ) ;
#9101 = VECTOR ( 'NONE', #9567, 1000.000000000000000 ) ;
#9102 = AXIS2_PLACEMENT_3D ( 'NONE', #9204, #12386, #9074 ) ;
#9103 = ORIENTED_EDGE ( 'NONE', *, *, #5250, .F. ) ;
#9104 = CARTESIAN_POINT ( 'NONE',  ( 5.000000000000000000, -4.685197434473820088, 9.540979117872439019E-15 ) ) ;
#9105 = CARTESIAN_POINT ( 'NONE',  ( 76.03431729618309021, 6.123233995736675563E-16, -5.000000000000007994 ) ) ;
#9106 = VECTOR ( 'NONE', #22177, 1000.000000000000000 ) ;
#9107 = DIRECTION ( 'NONE',  ( -1.000000000000000000, -1.224606353822377258E-16, -0.000000000000000000 ) ) ;
#9108 = CARTESIAN_POINT ( 'NONE',  ( -24.75000000000000000, 29.50000000000000000, 14.00000000000000178 ) ) ;
#9109 = AXIS2_PLACEMENT_3D ( 'NONE', #16208, #21939, #20232 ) ;
#9110 = DIRECTION ( 'NONE',  ( 0.000000000000000000, 0.000000000000000000, 1.000000000000000000 ) ) ;
#9111 = DIRECTION ( 'NONE',  ( -1.000000000000000000, -1.224606353822377258E-16, -0.000000000000000000 ) ) ;
#9112 = SURFACE_STYLE_FILL_AREA ( #18393 ) ;
#9113 = ORIENTED_EDGE ( 'NONE', *, *, #6933, .T. ) ;
#9114 = ORIENTED_EDGE ( 'NONE', *, *, #11680, .T. ) ;
#9115 = CARTESIAN_POINT ( 'NONE',  ( -5.871322893124554021, 8.081182679343978492, 7.906742014460233392 ) ) ;
#9116 = EDGE_CURVE ( 'NONE', #2505, #230, #11788, .T. ) ;
#9117 = ORIENTED_EDGE ( 'NONE', *, *, #6248, .F. ) ;
#9118 = ADVANCED_FACE ( 'NONE', ( #8017 ), #4376, .T. ) ;
#9119 = ORIENTED_EDGE ( 'NONE', *, *, #9606, .T. ) ;
#9120 =( LENGTH_UNIT ( ) NAMED_UNIT ( * ) SI_UNIT ( .MILLI., .METRE. ) );
#9121 = VECTOR ( 'NONE', #19115, 1000.000000000000000 ) ;
#9122 = CONICAL_SURFACE ( 'NONE', #21204, 4.172000000000008590, 0.9599310885968742602 ) ;
#9123 = DIRECTION ( 'NONE',  ( 1.000000000000000000, 0.000000000000000000, 0.000000000000000000 ) ) ;
#9124 = CARTESIAN_POINT ( 'NONE',  ( 40.89823313241238623, -26.41789760203348081, 27.00000000000000000 ) ) ;
#9125 = CARTESIAN_POINT ( 'NONE',  ( 58.00000000000000000, 7.491529369508391930E-15, 0.000000000000000000 ) ) ;
#9126 = VECTOR ( 'NONE', #6655, 1000.000000000000000 ) ;
#9127 = TOROIDAL_SURFACE ( 'NONE', #22782, 5.999999999999999112, 1.000000000000000000 ) ;
#9128 = CARTESIAN_POINT ( 'NONE',  ( 85.63636363636365445, 7.491529369508391930E-15, 0.000000000000000000 ) ) ;
#9129 = DIRECTION ( 'NONE',  ( 0.000000000000000000, 0.000000000000000000, 1.000000000000000000 ) ) ;
#9130 = DIRECTION ( 'NONE',  ( -0.5000000000000003331, 0.8660254037844384856, 0.000000000000000000 ) ) ;
#9131 = FACE_OUTER_BOUND ( 'NONE', #301, .T. ) ;
#9132 = VERTEX_POINT ( 'NONE', #602 ) ;
#9133 = DIRECTION ( 'NONE',  ( 1.000000000000000000, 0.000000000000000000, 0.000000000000000000 ) ) ;
#9134 = CYLINDRICAL_SURFACE ( 'NONE', #935, 8.000000000000003553 ) ;
#9135 = DIRECTION ( 'NONE',  ( 1.000000000000000000, 0.000000000000000000, 0.000000000000000000 ) ) ;
#9136 = CYLINDRICAL_SURFACE ( 'NONE', #18887, 1.000000000000000888 ) ;
#9137 = VECTOR ( 'NONE', #15866, 1000.000000000000000 ) ;
#9138 = EDGE_CURVE ( 'NONE', #7050, #14193, #6086, .T. ) ;
#9139 = VECTOR ( 'NONE', #11358, 1000.000000000000000 ) ;
#9140 = CARTESIAN_POINT ( 'NONE',  ( 0.000000000000000000, -14.99147757894464306, 7.750000000000000000 ) ) ;
#9141 = DIRECTION ( 'NONE',  ( -0.000000000000000000, -0.000000000000000000, -1.000000000000000000 ) ) ;
#9142 = EDGE_CURVE ( 'NONE', #2036, #7070, #7458, .T. ) ;
#9143 = ORIENTED_EDGE ( 'NONE', *, *, #10101, .T. ) ;
#9144 = CARTESIAN_POINT ( 'NONE',  ( 0.2999999999999999889, 0.000000000000000000, 0.000000000000000000 ) ) ;
#9145 = VECTOR ( 'NONE', #11512, 1000.000000000000000 ) ;
#9146 = VERTEX_POINT ( 'NONE', #21212 ) ;
#9147 = CARTESIAN_POINT ( 'NONE',  ( 9.500000000000000000, 6.470877716354879437E-13, -10.05958914175814378 ) ) ;
#9148 = EDGE_CURVE ( 'NONE', #22869, #8004, #17054, .T. ) ;
#9149 = EDGE_CURVE ( 'NONE', #15083, #22027, #468, .T. ) ;
#9150 = ORIENTED_EDGE ( 'NONE', *, *, #14400, .F. ) ;
#9151 = CARTESIAN_POINT ( 'NONE',  ( 29.00000000000000355, -29.50000000000000000, -2.224999999999995204 ) ) ;
#9152 = VECTOR ( 'NONE', #4739, 1000.000000000000000 ) ;
#9153 = AXIS2_PLACEMENT_3D ( 'NONE', #5951, #17292, #19502 ) ;
#9154 = CARTESIAN_POINT ( 'NONE',  ( 7.937578510445358226, -3.514536757623690999, 12.49999999999999112 ) ) ;
#9155 = CARTESIAN_POINT ( 'NONE',  ( 40.00000000000000000, 29.49999999999999645, 0.000000000000000000 ) ) ;
#9156 = DIRECTION ( 'NONE',  ( 1.000000000000000000, 3.469446951953611822E-15, 0.000000000000000000 ) ) ;
#9157 = LINE ( 'NONE', #16603, #15315 ) ;
#9158 = CARTESIAN_POINT ( 'NONE',  ( -9.500000000000211386, 3.086737114211961064, -4.959589141758145026 ) ) ;
#9159 = ORIENTED_EDGE ( 'NONE', *, *, #8076, .T. ) ;
#9160 = VECTOR ( 'NONE', #15109, 1000.000000000000000 ) ;
#9161 = EDGE_LOOP ( 'NONE', ( #13380, #22308, #2442, #22277, #16660, #1194 ) ) ;
#9162 = DIRECTION ( 'NONE',  ( -1.000000000000000000, 0.000000000000000000, 0.000000000000000000 ) ) ;
#9163 = CARTESIAN_POINT ( 'NONE',  ( 0.000000000000000000, 0.000000000000000000, 12.50000000000000000 ) ) ;
#9164 = CIRCLE ( 'NONE', #4171, 14.72592346043842326 ) ;
#9165 = CARTESIAN_POINT ( 'NONE',  ( -31.74999999999995737, 0.000000000000000000, 0.000000000000000000 ) ) ;
#9166 = ADVANCED_FACE ( 'NONE', ( #723 ), #5960, .F. ) ;
#9167 = ORIENTED_EDGE ( 'NONE', *, *, #10499, .T. ) ;
#9168 = PLANE ( 'NONE',  #19196 ) ;
#9169 = DIRECTION ( 'NONE',  ( 0.000000000000000000, 0.000000000000000000, 1.000000000000000000 ) ) ;
#9170 = DIRECTION ( 'NONE',  ( -1.000000000000000000, -1.224606353822377258E-16, -0.000000000000000000 ) ) ;
#9171 = ORIENTED_EDGE ( 'NONE', *, *, #12174, .F. ) ;
#9172 = LINE ( 'NONE', #3561, #11439 ) ;
#9173 = DIRECTION ( 'NONE',  ( 0.000000000000000000, 0.000000000000000000, 1.000000000000000000 ) ) ;
#9174 = EDGE_CURVE ( 'NONE', #21420, #17969, #1656, .T. ) ;
#9175 = CARTESIAN_POINT ( 'NONE',  ( 1.999999999999994449, -45.00000000000000000, 0.02500000000000418554 ) ) ;
#9176 = ADVANCED_FACE ( 'NONE', ( #6202 ), #9836, .F. ) ;
#9177 = VECTOR ( 'NONE', #9471, 1000.000000000000000 ) ;
#9178 =( GEOMETRIC_REPRESENTATION_CONTEXT ( 3 ) GLOBAL_UNCERTAINTY_ASSIGNED_CONTEXT ( ( #9598 ) ) GLOBAL_UNIT_ASSIGNED_CONTEXT ( ( #20708, #18649, #11281 ) ) REPRESENTATION_CONTEXT ( 'NONE', 'WORKASPACE' ) );
#9179 = CARTESIAN_POINT ( 'NONE',  ( 7.022953521754877748, 5.102474405760673903, 4.833165578109188232 ) ) ;
#9180 = ORIENTED_EDGE ( 'NONE', *, *, #4799, .T. ) ;
#9181 = VERTEX_POINT ( 'NONE', #7884 ) ;
#9182 = AXIS2_PLACEMENT_3D ( 'NONE', #23739, #8357, #7008 ) ;
#9183 = ORIENTED_EDGE ( 'NONE', *, *, #6631, .T. ) ;
#9184 = VECTOR ( 'NONE', #16020, 1000.000000000000000 ) ;
#9185 = ORIENTED_EDGE ( 'NONE', *, *, #5504, .F. ) ;
#9186 = CARTESIAN_POINT ( 'NONE',  ( 0.000000000000000000, 11.37860023611358962, -13.78561139983841599 ) ) ;
#9187 = CARTESIAN_POINT ( 'NONE',  ( -6.822232771736904647E-13, 9.988891130263535700, 9.706742014460232326 ) ) ;
#9188 = ORIENTED_EDGE ( 'NONE', *, *, #15903, .T. ) ;
#9189 = ORIENTED_EDGE ( 'NONE', *, *, #9707, .F. ) ;
#9190 = CIRCLE ( 'NONE', #4145, 10.02592346138681201 ) ;
#9191 = CARTESIAN_POINT ( 'NONE',  ( 0.000000000000000000, 0.000000000000000000, 12.50000000000000000 ) ) ;
#9192 = VERTEX_POINT ( 'NONE', #9964 ) ;
#9193 = DIRECTION ( 'NONE',  ( -0.4828336235133042775, 0.8757121056631643752, 0.000000000000000000 ) ) ;
#9194 = CARTESIAN_POINT ( 'NONE',  ( 65.27272727272728048, 4.172000000000015696, 5.109226446042767468E-16 ) ) ;
#9195 = PRODUCT_DEFINITION_FORMATION_WITH_SPECIFIED_SOURCE ( 'ANY', '', #10591, .NOT_KNOWN. ) ;
#9196 = EDGE_CURVE ( 'NONE', #20146, #16881, #20860, .T. ) ;
#9197 = AXIS2_PLACEMENT_3D ( 'NONE', #20069, #3349, #10769 ) ;
#9198 = CARTESIAN_POINT ( 'NONE',  ( -40.50000000000000000, -51.00000000000000711, 12.50000000000000000 ) ) ;
#9199 = DIRECTION ( 'NONE',  ( -1.000000000000000000, 0.000000000000000000, 0.000000000000000000 ) ) ;
#9200 = VECTOR ( 'NONE', #767, 1000.000000000000114 ) ;
#9201 = CARTESIAN_POINT ( 'NONE',  ( 23.00000000000000000, -2.110835303355205639, -14.05523051341068097 ) ) ;
#9202 = ADVANCED_FACE ( 'NONE', ( #15092 ), #6729, .T. ) ;
#9203 = FACE_BOUND ( 'NONE', #21275, .T. ) ;
#9204 = CARTESIAN_POINT ( 'NONE',  ( -41.00000000000000000, 6.000000000000000888, 10.49999999999999822 ) ) ;
#9205 = LINE ( 'NONE', #13104, #7502 ) ;
#9206 = CARTESIAN_POINT ( 'NONE',  ( -14.98952570844870102, 0.6468970097546546949, -9.483487670324119989 ) ) ;
#9207 = VERTEX_POINT ( 'NONE', #466 ) ;
#9208 = EDGE_CURVE ( 'NONE', #9833, #1756, #19391, .T. ) ;
#9209 = CARTESIAN_POINT ( 'NONE',  ( -7.022953521755574080, 5.102474405759713783, 9.433165578109189653 ) ) ;
#9210 = EDGE_LOOP ( 'NONE', ( #14314, #19219, #22224, #14913 ) ) ;
#9211 = AXIS2_PLACEMENT_3D ( 'NONE', #3694, #2099, #519 ) ;
#9212 = APPLICATION_PROTOCOL_DEFINITION ( 'draft international standard', 'automotive_design', 1998, #453 ) ;
#9213 = DIRECTION ( 'NONE',  ( 0.000000000000000000, -1.000000000000000000, 0.000000000000000000 ) ) ;
#9214 = ORIENTED_EDGE ( 'NONE', *, *, #16101, .T. ) ;
#9215 = EDGE_LOOP ( 'NONE', ( #17313, #16994, #5425, #12479 ) ) ;
#9216 = LINE ( 'NONE', #19973, #15378 ) ;
#9217 = CARTESIAN_POINT ( 'NONE',  ( 7.022953521754877748, 5.102474405760673903, -8.833165578109190008 ) ) ;
#9218 = ORIENTED_EDGE ( 'NONE', *, *, #20515, .T. ) ;
#9219 = DIRECTION ( 'NONE',  ( 0.000000000000000000, -0.5150380749100544886, -0.8571673007021121116 ) ) ;
#9220 = CARTESIAN_POINT ( 'NONE',  ( 23.00000000000000000, -13.66196005206961850, 2.131329562388824428 ) ) ;
#9221 = DIRECTION ( 'NONE',  ( -1.000000000000000000, -1.224606353822377258E-16, -0.000000000000000000 ) ) ;
#9222 = DIRECTION ( 'NONE',  ( 0.000000000000000000, 0.000000000000000000, -1.000000000000000000 ) ) ;
#9223 = LINE ( 'NONE', #18381, #16669 ) ;
#9224 = CARTESIAN_POINT ( 'NONE',  ( -23.85000000000000142, 15.03999999999999737, 0.000000000000000000 ) ) ;
#9225 = ORIENTED_EDGE ( 'NONE', *, *, #18122, .T. ) ;
#9226 = EDGE_CURVE ( 'NONE', #17379, #13080, #17633, .T. ) ;
#9227 = VERTEX_POINT ( 'NONE', #13262 ) ;
#9228 = CARTESIAN_POINT ( 'NONE',  ( -9.499999999999790390, -3.086737114213257804, -7.159589141758144315 ) ) ;
#9229 = DIRECTION ( 'NONE',  ( 0.000000000000000000, 0.000000000000000000, 1.000000000000000000 ) ) ;
#9230 = CARTESIAN_POINT ( 'NONE',  ( -14.99999999999999822, 0.000000000000000000, 27.00000000000000000 ) ) ;
#9231 = FILL_AREA_STYLE_COLOUR ( '', #956 ) ;
#9232 = ADVANCED_FACE ( 'NONE', ( #4006 ), #114, .T. ) ;
#9233 = CARTESIAN_POINT ( 'NONE',  ( -34.00000000000000000, 3.999999999999999112, 9.500000000000000000 ) ) ;
#9234 = LINE ( 'NONE', #20955, #5578 ) ;
#9235 = ADVANCED_FACE ( 'NONE', ( #18899 ), #9605, .F. ) ;
#9236 = DIRECTION ( 'NONE',  ( 1.000000000000000000, 0.000000000000000000, 0.000000000000000000 ) ) ;
#9237 = ORIENTED_EDGE ( 'NONE', *, *, #6046, .F. ) ;
#9238 = ORIENTED_EDGE ( 'NONE', *, *, #8463, .T. ) ;
#9239 = CARTESIAN_POINT ( 'NONE',  ( 5.871322893123449127, 8.081182679344781405, 9.506742014460231260 ) ) ;
#9240 = ORIENTED_EDGE ( 'NONE', *, *, #20385, .F. ) ;
#9241 = ORIENTED_EDGE ( 'NONE', *, *, #17445, .F. ) ;
#9242 = SHAPE_REPRESENTATION_RELATIONSHIP ( 'NONE' , 'NONE' ,  #19247, #9857 ) ;
#9243 = VERTEX_POINT ( 'NONE', #19134 ) ;
#9244 = FACE_OUTER_BOUND ( 'NONE', #11931, .T. ) ;
#9245 = CARTESIAN_POINT ( 'NONE',  ( -9.499999999999799272, -3.086737114213243593, 9.159589141758143427 ) ) ;
#9246 = DIRECTION ( 'NONE',  ( -0.000000000000000000, -0.000000000000000000, -1.000000000000000000 ) ) ;
#9247 = DIRECTION ( 'NONE',  ( -1.000000000000000000, 0.000000000000000000, 0.000000000000000000 ) ) ;
#9248 = ADVANCED_FACE ( 'NONE', ( #2412 ), #21458, .F. ) ;
#9249 = VERTEX_POINT ( 'NONE', #2910 ) ;
#9250 = EDGE_CURVE ( 'NONE', #5468, #7070, #4749, .T. ) ;
#9251 = DIRECTION ( 'NONE',  ( 0.000000000000000000, 1.000000000000000000, 0.000000000000000000 ) ) ;
#9252 = CARTESIAN_POINT ( 'NONE',  ( -34.00000000000000000, -3.851859888774471706E-31, 9.500000000000000000 ) ) ;
#9253 = LINE ( 'NONE', #1936, #16819 ) ;
#9254 = FACE_OUTER_BOUND ( 'NONE', #2383, .T. ) ;
#9255 = CARTESIAN_POINT ( 'NONE',  ( -5.871322893123449127, -8.081182679344781405, -11.35958914175814272 ) ) ;
#9256 = CARTESIAN_POINT ( 'NONE',  ( -36.00000000000001421, 50.99999999999999289, 12.50000000000000000 ) ) ;
#9257 = VECTOR ( 'NONE', #3088, 1000.000000000000227 ) ;
#9258 = CONICAL_SURFACE ( 'NONE', #10839, 4.249999999999993783, 1.029744258676653645 ) ;
#9259 = ORIENTED_EDGE ( 'NONE', *, *, #8581, .F. ) ;
#9260 = FACE_OUTER_BOUND ( 'NONE', #4618, .T. ) ;
#9261 = ORIENTED_EDGE ( 'NONE', *, *, #15427, .F. ) ;
#9262 = DIRECTION ( 'NONE',  ( 0.000000000000000000, 0.000000000000000000, 1.000000000000000000 ) ) ;
#9263 = VERTEX_POINT ( 'NONE', #23172 ) ;
#9264 =( NAMED_UNIT ( * ) PLANE_ANGLE_UNIT ( ) SI_UNIT ( $, .RADIAN. ) );
#9265 = FACE_OUTER_BOUND ( 'NONE', #19351, .T. ) ;
#9266 = DIRECTION ( 'NONE',  ( 0.000000000000000000, -1.000000000000000000, 0.000000000000000000 ) ) ;
#9267 = PRODUCT_RELATED_PRODUCT_CATEGORY ( 'part', '', ( #23684 ) ) ;
#9268 = CIRCLE ( 'NONE', #13573, 40.00000000000000000 ) ;
#9269 = CARTESIAN_POINT ( 'NONE',  ( 0.000000000000000000, 0.000000000000000000, 0.000000000000000000 ) ) ;
#9270 = CARTESIAN_POINT ( 'NONE',  ( 7.685661446561619314, 5.583959896779020049, -6.259589141758143960 ) ) ;
#9271 = ORIENTED_EDGE ( 'NONE', *, *, #11448, .T. ) ;
#9272 = ORIENTED_EDGE ( 'NONE', *, *, #1728, .F. ) ;
#9273 = CARTESIAN_POINT ( 'NONE',  ( -31.74999999999995737, 0.000000000000000000, 0.000000000000000000 ) ) ;
#9274 = ADVANCED_FACE ( 'NONE', ( #21584 ), #16201, .F. ) ;
#9275 = ADVANCED_FACE ( 'NONE', ( #6932 ), #14120, .F. ) ;
#9276 = VERTEX_POINT ( 'NONE', #5093 ) ;
#9277 = CARTESIAN_POINT ( 'NONE',  ( 42.00000000000000000, -6.000000000000015099, 10.49999999999999822 ) ) ;
#9278 = VERTEX_POINT ( 'NONE', #16066 ) ;
#9279 = CLOSED_SHELL ( 'NONE', ( #19053, #2235, #15459, #14241, #23984, #12788, #23484, #21195, #21592, #23763, #12618, #5191, #5886, #17329, #9202, #7376, #6621, #3512, #13614, #17977, #11564, #17181, #9657, #3815, #3931, #10041, #9388, #454, #2268, #18790, #18937, #23366, #14166, #5280, #22526, #17589, #1586, #343, #19646, #5742, #2914, #9363, #16188, #17973, #18563, #597, #7917, #8880, #15424, #5017, #22199, #20695 ) ) ;
#9280 = SPHERICAL_SURFACE ( 'NONE', #17639, 1.000000000000000000 ) ;
#9281 = DIRECTION ( 'NONE',  ( -0.000000000000000000, -0.000000000000000000, -1.000000000000000000 ) ) ;
#9282 = FACE_OUTER_BOUND ( 'NONE', #18700, .T. ) ;
#9283 = ORIENTED_EDGE ( 'NONE', *, *, #12704, .T. ) ;
#9284 = DIRECTION ( 'NONE',  ( 0.000000000000000000, 0.000000000000000000, 1.000000000000000000 ) ) ;
#9285 = CARTESIAN_POINT ( 'NONE',  ( -10.00000000000000000, 0.000000000000000000, 0.000000000000000000 ) ) ;
#9286 = CARTESIAN_POINT ( 'NONE',  ( -24.75000000000000000, -29.50000000000000000, -2.224999999999995204 ) ) ;
#9287 = PLANE ( 'NONE',  #19375 ) ;
#9288 = CARTESIAN_POINT ( 'NONE',  ( -2.682529543900285862, 8.255977015246234174, 7.233165578109188587 ) ) ;
#9289 = ORIENTED_EDGE ( 'NONE', *, *, #11157, .T. ) ;
#9290 = VERTEX_POINT ( 'NONE', #6691 ) ;
#9291 = EDGE_CURVE ( 'NONE', #9099, #7332, #21701, .T. ) ;
#9292 = ORIENTED_EDGE ( 'NONE', *, *, #11558, .T. ) ;
#9293 = DIRECTION ( 'NONE',  ( 0.5735764363510424957, 0.8191520442889943521, 0.000000000000000000 ) ) ;
#9294 = EDGE_CURVE ( 'NONE', #6856, #4207, #23302, .T. ) ;
#9295 = DIRECTION ( 'NONE',  ( -1.000000000000000000, -1.224606353822377258E-16, -0.000000000000000000 ) ) ;
#9296 = ORIENTED_EDGE ( 'NONE', *, *, #659, .F. ) ;
#9297 = EDGE_CURVE ( 'NONE', #732, #5422, #16461, .T. ) ;
#9298 = EDGE_CURVE ( 'NONE', #2368, #3703, #9422, .T. ) ;
#9299 = EDGE_CURVE ( 'NONE', #15211, #17944, #12291, .T. ) ;
#9300 = CARTESIAN_POINT ( 'NONE',  ( 0.000000000000000000, 15.03999999999999737, 2.200000000000000178 ) ) ;
#9301 = ORIENTED_EDGE ( 'NONE', *, *, #14272, .T. ) ;
#9302 =( REPRESENTATION_RELATIONSHIP ('NONE','NONE', #21748, #852 ) REPRESENTATION_RELATIONSHIP_WITH_TRANSFORMATION ( #21016 )SHAPE_REPRESENTATION_RELATIONSHIP( ) );
#9303 = CARTESIAN_POINT ( 'NONE',  ( -29.00000000000000000, -29.49999999999999645, 12.00000000000000000 ) ) ;
#9304 = CARTESIAN_POINT ( 'NONE',  ( 0.000000000000000000, -13.66196005206961850, 2.131329562388824428 ) ) ;
#9305 = LINE ( 'NONE', #10666, #6079 ) ;
#9306 = DIRECTION ( 'NONE',  ( -1.000000000000000000, -1.224606353822377258E-16, -0.000000000000000000 ) ) ;
#9307 = CARTESIAN_POINT ( 'NONE',  ( 24.75000000000000355, 29.50000000000000000, -3.000000000000000000 ) ) ;
#9308 = CARTESIAN_POINT ( 'NONE',  ( 23.00000000000000000, -14.80154252341789700, -10.02147513732837680 ) ) ;
#9309 = DIRECTION ( 'NONE',  ( -0.000000000000000000, 1.000000000000000000, -0.000000000000000000 ) ) ;
#9310 = EDGE_LOOP ( 'NONE', ( #13250, #11798, #770, #5971, #18797 ) ) ;
#9311 = CARTESIAN_POINT ( 'NONE',  ( 2.935661446561383503, 9.035036904804158553, 10.45958914175814414 ) ) ;
#9312 = ORIENTED_EDGE ( 'NONE', *, *, #21074, .F. ) ;
#9313 = AXIS2_PLACEMENT_3D ( 'NONE', #17772, #4487, #2644 ) ;
#9314 = APPLICATION_PROTOCOL_DEFINITION ( 'draft international standard', 'automotive_design', 1998, #20101 ) ;
#9315 = EDGE_CURVE ( 'NONE', #12921, #21260, #6577, .T. ) ;
#9316 = ORIENTED_EDGE ( 'NONE', *, *, #3636, .T. ) ;
#9317 = ORIENTED_EDGE ( 'NONE', *, *, #8013, .F. ) ;
#9318 = DIRECTION ( 'NONE',  ( 0.000000000000000000, -0.4999999999999992784, 0.8660254037844390407 ) ) ;
#9319 = CARTESIAN_POINT ( 'NONE',  ( 8.680847955711007202, 5.912916378492122225E-13, -8.633165578109188942 ) ) ;
#9320 = DIRECTION ( 'NONE',  ( 0.000000000000000000, 1.000000000000000000, 0.000000000000000000 ) ) ;
#9321 = VERTEX_POINT ( 'NONE', #19761 ) ;
#9322 = DIRECTION ( 'NONE',  ( 1.000000000000000000, 0.000000000000000000, 0.000000000000000000 ) ) ;
#9323 = DIRECTION ( 'NONE',  ( -1.000000000000000000, 0.000000000000000000, 0.000000000000000000 ) ) ;
#9324 = CARTESIAN_POINT ( 'NONE',  ( 29.00000000000000000, -29.50000000000000355, 11.50000000000000000 ) ) ;
#9325 = EDGE_CURVE ( 'NONE', #2764, #21134, #21136, .T. ) ;
#9326 = DIRECTION ( 'NONE',  ( 0.000000000000000000, 0.000000000000000000, 1.000000000000000000 ) ) ;
#9327 = ADVANCED_FACE ( 'NONE', ( #10457 ), #17916, .F. ) ;
#9328 = DIRECTION ( 'NONE',  ( 0.000000000000000000, -1.000000000000000000, 0.000000000000000000 ) ) ;
#9329 = VERTEX_POINT ( 'NONE', #14240 ) ;
#9330 = LINE ( 'NONE', #7493, #504 ) ;
#9331 = ORIENTED_EDGE ( 'NONE', *, *, #7253, .T. ) ;
#9332 = DIRECTION ( 'NONE',  ( 0.000000000000000000, 0.000000000000000000, -1.000000000000000000 ) ) ;
#9333 = CARTESIAN_POINT ( 'NONE',  ( -7.685661446562381371, 5.583959896777970222, -8.859589141758144493 ) ) ;
#9334 = DIRECTION ( 'NONE',  ( -1.000000000000000000, 0.000000000000000000, 0.000000000000000000 ) ) ;
#9335 = CARTESIAN_POINT ( 'NONE',  ( 14.80736872429922357, 4.130115634539733627, -8.564444421911364458 ) ) ;
#9336 = CARTESIAN_POINT ( 'NONE',  ( 35.99999999999999289, -51.00000000000000711, 12.50000000000000000 ) ) ;
#9337 = CARTESIAN_POINT ( 'NONE',  ( 7.937578510445243651, -3.514536757623948127, -12.49999999999998046 ) ) ;
#9338 = DIRECTION ( 'NONE',  ( 1.000000000000000000, 0.000000000000000000, 0.000000000000000000 ) ) ;
#9339 = ORIENTED_EDGE ( 'NONE', *, *, #17974, .F. ) ;
#9340 = ORIENTED_EDGE ( 'NONE', *, *, #22861, .T. ) ;
#9341 = EDGE_LOOP ( 'NONE', ( #21300, #2208, #3025, #1628, #12574 ) ) ;
#9342 = EDGE_LOOP ( 'NONE', ( #3267, #946 ) ) ;
#9343 =( NAMED_UNIT ( * ) SI_UNIT ( $, .STERADIAN. ) SOLID_ANGLE_UNIT ( ) );
#9344 = ORIENTED_EDGE ( 'NONE', *, *, #8473, .T. ) ;
#9345 = DIRECTION ( 'NONE',  ( 0.000000000000000000, 0.000000000000000000, -1.000000000000000000 ) ) ;
#9346 = DIRECTION ( 'NONE',  ( 0.000000000000000000, -1.000000000000000000, 0.000000000000000000 ) ) ;
#9347 = DIRECTION ( 'NONE',  ( -1.000000000000000000, 0.000000000000000000, 0.000000000000000000 ) ) ;
#9348 = EDGE_CURVE ( 'NONE', #12511, #6174, #12407, .T. ) ;
#9349 = DIRECTION ( 'NONE',  ( -0.000000000000000000, -0.000000000000000000, 1.000000000000000000 ) ) ;
#9350 = ORIENTED_EDGE ( 'NONE', *, *, #22737, .F. ) ;
#9351 = DIRECTION ( 'NONE',  ( -1.000000000000000000, -1.224606353822377258E-16, -0.000000000000000000 ) ) ;
#9352 = CARTESIAN_POINT ( 'NONE',  ( -17.49232137458055192, 9.205685982891283814, 2.395442301836276933 ) ) ;
#9353 = CIRCLE ( 'NONE', #434, 9.999999999999998224 ) ;
#9354 = CYLINDRICAL_SURFACE ( 'NONE', #948, 5.000000000000000888 ) ;
#9355 = PRODUCT ( 'Housing Seal', 'Housing Seal', '', ( #7606 ) ) ;
#9356 = VERTEX_POINT ( 'NONE', #12509 ) ;
#9357 = CARTESIAN_POINT ( 'NONE',  ( -2.024999999999999911, 45.00000000000000000, -3.000000000000000000 ) ) ;
#9358 = ORIENTED_EDGE ( 'NONE', *, *, #12454, .F. ) ;
#9359 = CARTESIAN_POINT ( 'NONE',  ( 0.000000000000000000, 0.000000000000000000, 15.00000000000000178 ) ) ;
#9360 = ORIENTED_EDGE ( 'NONE', *, *, #21450, .F. ) ;
#9361 = DIRECTION ( 'NONE',  ( -0.000000000000000000, 0.000000000000000000, 1.000000000000000000 ) ) ;
#9362 = CARTESIAN_POINT ( 'NONE',  ( -19.84999999999999787, -16.67999999999985761, 14.50000000000000000 ) ) ;
#9363 = ADVANCED_FACE ( 'NONE', ( #1326 ), #19981, .T. ) ;
#9364 = EDGE_LOOP ( 'NONE', ( #23364, #2063, #16919, #11256 ) ) ;
#9365 = DIRECTION ( 'NONE',  ( 0.000000000000000000, 0.000000000000000000, 1.000000000000000000 ) ) ;
#9366 = CARTESIAN_POINT ( 'NONE',  ( 30.44534269664590553, 40.40463133211080304, 11.00000000000000000 ) ) ;
#9367 = LINE ( 'NONE', #11446, #4951 ) ;
#9368 = EDGE_CURVE ( 'NONE', #18644, #21399, #10987, .T. ) ;
#9369 = CARTESIAN_POINT ( 'NONE',  ( 5.078177448618336420, 0.000000000000000000, 10.94716442891539643 ) ) ;
#9370 = AXIS2_PLACEMENT_3D ( 'NONE', #5079, #23644, #14577 ) ;
#9371 = ADVANCED_FACE ( 'NONE', ( #4631, #12033 ), #13002, .F. ) ;
#9372 = AXIS2_PLACEMENT_3D ( 'NONE', #4354, #7854, #22905 ) ;
#9373 = CARTESIAN_POINT ( 'NONE',  ( 9.500000000000000000, 6.470877716354879437E-13, -8.059589141758143782 ) ) ;
#9374 = ORIENTED_EDGE ( 'NONE', *, *, #21760, .F. ) ;
#9375 = DIRECTION ( 'NONE',  ( 1.000000000000000000, 0.000000000000000000, 0.000000000000000000 ) ) ;
#9376 = CARTESIAN_POINT ( 'NONE',  ( 9.499999999999790390, 3.086737114213260025, 11.30674201446023197 ) ) ;
#9377 = ORIENTED_EDGE ( 'NONE', *, *, #19415, .F. ) ;
#9378 = DIRECTION ( 'NONE',  ( 0.8191520442889927978, 5.579613378627572123E-14, -0.5735764363510448272 ) ) ;
#9379 = EDGE_LOOP ( 'NONE', ( #18343, #3485, #18740, #1631 ) ) ;
#9380 = DIRECTION ( 'NONE',  ( -0.000000000000000000, -0.000000000000000000, -1.000000000000000000 ) ) ;
#9381 = DIRECTION ( 'NONE',  ( -1.000000000000000000, 0.000000000000000000, 0.000000000000000000 ) ) ;
#9382 = CARTESIAN_POINT ( 'NONE',  ( 40.77574956473004164, 27.49633847812775755, 0.000000000000000000 ) ) ;
#9383 = CIRCLE ( 'NONE', #19173, 20.85000000000000853 ) ;
#9384 = ORIENTED_EDGE ( 'NONE', *, *, #7404, .T. ) ;
#9385 = DIRECTION ( 'NONE',  ( 0.000000000000000000, 0.000000000000000000, -1.000000000000000000 ) ) ;
#9386 = DIRECTION ( 'NONE',  ( -1.000000000000000000, -0.000000000000000000, -0.000000000000000000 ) ) ;
#9387 = CIRCLE ( 'NONE', #8642, 1.000000000000000000 ) ;
#9388 = ADVANCED_FACE ( 'NONE', ( #22289 ), #16547, .T. ) ;
#9389 = DIRECTION ( 'NONE',  ( 0.000000000000000000, 0.000000000000000000, 1.000000000000000000 ) ) ;
#9390 = CARTESIAN_POINT ( 'NONE',  ( 0.000000000000000000, 45.00000000000000000, -2.974999999999996092 ) ) ;
#9391 = EDGE_LOOP ( 'NONE', ( #15078, #19364, #5347, #23669 ) ) ;
#9392 = EDGE_CURVE ( 'NONE', #22141, #13616, #16305, .T. ) ;
#9393 = ORIENTED_EDGE ( 'NONE', *, *, #8118, .F. ) ;
#9394 = ADVANCED_FACE ( 'NONE', ( #23766 ), #1456, .T. ) ;
#9395 = ORIENTED_EDGE ( 'NONE', *, *, #5638, .T. ) ;
#9396 = EDGE_LOOP ( 'NONE', ( #22733, #6543, #24059, #7018 ) ) ;
#9397 = CARTESIAN_POINT ( 'NONE',  ( -36.00000000000000711, -51.00000000000000711, 12.50000000000000000 ) ) ;
#9398 = LINE ( 'NONE', #3935, #6026 ) ;
#9399 = CARTESIAN_POINT ( 'NONE',  ( 74.57977184163763695, -5.000000000000000888, 6.123233995736776143E-16 ) ) ;
#9400 = ORIENTED_EDGE ( 'NONE', *, *, #14454, .T. ) ;
#9401 = AXIS2_PLACEMENT_3D ( 'NONE', #18744, #22293, #22540 ) ;
#9402 = VECTOR ( 'NONE', #8131, 1000.000000000000000 ) ;
#9403 = CIRCLE ( 'NONE', #14491, 50.00000000000000000 ) ;
#9404 = VECTOR ( 'NONE', #4380, 1000.000000000000000 ) ;
#9405 = EDGE_LOOP ( 'NONE', ( #22404, #13818, #20983, #7586 ) ) ;
#9406 = DIRECTION ( 'NONE',  ( -1.000000000000000000, -1.224606353822377258E-16, -0.000000000000000000 ) ) ;
#9407 = AXIS2_PLACEMENT_3D ( 'NONE', #5157, #4821, #12587 ) ;
#9408 = AXIS2_PLACEMENT_3D ( 'NONE', #16730, #16500, #18588 ) ;
#9409 = CARTESIAN_POINT ( 'NONE',  ( 62.36363636363636687, 7.491529369508391930E-15, 0.000000000000000000 ) ) ;
#9410 = DIRECTION ( 'NONE',  ( -1.000000000000000000, 0.000000000000000000, 0.000000000000000000 ) ) ;
#9411 = CARTESIAN_POINT ( 'NONE',  ( -31.74999999999995737, 0.000000000000000000, 0.000000000000000000 ) ) ;
#9412 = EDGE_CURVE ( 'NONE', #22424, #14048, #8273, .T. ) ;
#9413 = FACE_BOUND ( 'NONE', #23542, .T. ) ;
#9414 = ORIENTED_EDGE ( 'NONE', *, *, #1078, .F. ) ;
#9415 = DIRECTION ( 'NONE',  ( 0.000000000000000000, 0.000000000000000000, 1.000000000000000000 ) ) ;
#9416 = LINE ( 'NONE', #2248, #6364 ) ;
#9417 = DIRECTION ( 'NONE',  ( -1.000000000000000000, 0.000000000000000000, 0.000000000000000000 ) ) ;
#9418 = EDGE_LOOP ( 'NONE', ( #7146, #5417, #14273, #8429 ) ) ;
#9419 = ORIENTED_EDGE ( 'NONE', *, *, #16535, .T. ) ;
#9420 = CARTESIAN_POINT ( 'NONE',  ( -8.680847955711007202, -5.923547351154968927E-13, 3.633165578109188054 ) ) ;
#9421 = ORIENTED_EDGE ( 'NONE', *, *, #6689, .T. ) ;
#9422 = CIRCLE ( 'NONE', #6337, 5.000000000000007994 ) ;
#9423 = EDGE_CURVE ( 'NONE', #12017, #25, #893, .T. ) ;
#9424 = CIRCLE ( 'NONE', #19611, 9.999999999999998224 ) ;
#9425 = EDGE_CURVE ( 'NONE', #15969, #8536, #9100, .T. ) ;
#9426 = AXIS2_PLACEMENT_3D ( 'NONE', #4139, #15802, #7877 ) ;
#9427 = ITEM_DEFINED_TRANSFORMATION ( 'NONE', 'NONE', #3759,  #8005 ) ;
#9428 = AXIS2_PLACEMENT_3D ( 'NONE', #7289, #3398, #1686 ) ;
#9429 = VECTOR ( 'NONE', #11197, 1000.000000000000000 ) ;
#9430 = ORIENTED_EDGE ( 'NONE', *, *, #10628, .F. ) ;
#9431 = EDGE_LOOP ( 'NONE', ( #18234, #9117, #341, #21988 ) ) ;
#9432 = LINE ( 'NONE', #15163, #11001 ) ;
#9433 = CARTESIAN_POINT ( 'NONE',  ( -9.500000000000211386, 3.086737114211961064, -2.959589141758143249 ) ) ;
#9434 = AXIS2_PLACEMENT_3D ( 'NONE', #3320, #6274, #3189 ) ;
#9435 = PLANE ( 'NONE',  #15725 ) ;
#9436 = ORIENTED_EDGE ( 'NONE', *, *, #17295, .T. ) ;
#9437 = LINE ( 'NONE', #11031, #17296 ) ;
#9438 = DIRECTION ( 'NONE',  ( -0.000000000000000000, -0.000000000000000000, -1.000000000000000000 ) ) ;
#9439 = APPLICATION_CONTEXT ( 'automotive_design' ) ;
#9440 = LINE ( 'NONE', #7491, #10824 ) ;
#9441 = ORIENTED_EDGE ( 'NONE', *, *, #20267, .T. ) ;
#9442 = CYLINDRICAL_SURFACE ( 'NONE', #20375, 9.500000000000000000 ) ;
#9443 = CIRCLE ( 'NONE', #23119, 23.85000000000000497 ) ;
#9444 = AXIS2_PLACEMENT_3D ( 'NONE', #1210, #22072, #21710 ) ;
#9445 = DIRECTION ( 'NONE',  ( -1.000000000000000000, -1.224606353822377258E-16, -0.000000000000000000 ) ) ;
#9446 = DIRECTION ( 'NONE',  ( -0.000000000000000000, 0.000000000000000000, 1.000000000000000000 ) ) ;
#9447 = AXIS2_PLACEMENT_3D ( 'NONE', #18128, #19940, #20190 ) ;
#9448 = DIRECTION ( 'NONE',  ( 0.000000000000000000, -1.000000000000000000, 0.000000000000000000 ) ) ;
#9449 = DIRECTION ( 'NONE',  ( 0.000000000000000000, 0.000000000000000000, 1.000000000000000000 ) ) ;
#9450 = AXIS2_PLACEMENT_3D ( 'NONE', #14921, #66, #24091 ) ;
#9451 = EDGE_CURVE ( 'NONE', #886, #7845, #14508, .T. ) ;
#9452 = AXIS2_PLACEMENT_3D ( 'NONE', #9642, #20401, #22491 ) ;
#9453 = DIRECTION ( 'NONE',  ( -0.000000000000000000, -0.000000000000000000, -1.000000000000000000 ) ) ;
#9454 = CARTESIAN_POINT ( 'NONE',  ( -8.680847955710813579, -2.820578480814257549, -11.73316557810918859 ) ) ;
#9455 = VECTOR ( 'NONE', #1111, 999.9999999999998863 ) ;
#9456 = DIRECTION ( 'NONE',  ( -1.000000000000000000, -0.000000000000000000, -0.000000000000000000 ) ) ;
#9457 = ORIENTED_EDGE ( 'NONE', *, *, #2880, .F. ) ;
#9458 = ORIENTED_EDGE ( 'NONE', *, *, #8187, .F. ) ;
#9459 = CARTESIAN_POINT ( 'NONE',  ( -7.685661446562381371, 5.583959896777970222, 4.006742014460233925 ) ) ;
#9460 = EDGE_CURVE ( 'NONE', #2565, #21660, #24002, .T. ) ;
#9461 = VERTEX_POINT ( 'NONE', #8865 ) ;
#9462 = EDGE_CURVE ( 'NONE', #16379, #23250, #2434, .T. ) ;
#9463 = EDGE_LOOP ( 'NONE', ( #23242, #3793 ) ) ;
#9464 = VERTEX_POINT ( 'NONE', #10806 ) ;
#9465 = DIRECTION ( 'NONE',  ( -1.000000000000000000, 0.000000000000000000, -0.000000000000000000 ) ) ;
#9466 = CIRCLE ( 'NONE', #13779, 14.72592346043842326 ) ;
#9467 = CIRCLE ( 'NONE', #8701, 12.73082370883260594 ) ;
#9468 = AXIS2_PLACEMENT_3D ( 'NONE', #207, #3739, #2376 ) ;
#9469 = VECTOR ( 'NONE', #19926, 1000.000000000000000 ) ;
#9470 = DIRECTION ( 'NONE',  ( -0.9160001545545232160, 0.4011779117250717785, -0.000000000000000000 ) ) ;
#9471 = DIRECTION ( 'NONE',  ( -1.000000000000000000, -0.000000000000000000, -0.000000000000000000 ) ) ;
#9472 = DIRECTION ( 'NONE',  ( 0.000000000000000000, -1.000000000000000000, 0.000000000000000000 ) ) ;
#9473 = AXIS2_PLACEMENT_3D ( 'NONE', #672, #8466, #19343 ) ;
#9474 = AXIS2_PLACEMENT_3D ( 'NONE', #15540, #15061, #4475 ) ;
#9475 = CARTESIAN_POINT ( 'NONE',  ( -9.500000000000220268, 3.086737114211950406, -10.95958914175814236 ) ) ;
#9476 = ORIENTED_EDGE ( 'NONE', *, *, #10790, .F. ) ;
#9477 = DIRECTION ( 'NONE',  ( -1.000000000000000000, -0.000000000000000000, 0.000000000000000000 ) ) ;
#9478 = SURFACE_STYLE_FILL_AREA ( #2053 ) ;
#9479 = FACE_OUTER_BOUND ( 'NONE', #921, .T. ) ;
#9480 = CARTESIAN_POINT ( 'NONE',  ( -17.38700629636782580, 8.908123924593990495, -3.336041480784321056 ) ) ;
#9481 = CARTESIAN_POINT ( 'NONE',  ( 23.00000000000000000, -11.55437235128772500, -1.752358929577761515 ) ) ;
#9482 = ORIENTED_EDGE ( 'NONE', *, *, #1782, .T. ) ;
#9483 = CARTESIAN_POINT ( 'NONE',  ( 2.682529543900284974, -8.255977015246234174, -6.233165578109188587 ) ) ;
#9484 = DIRECTION ( 'NONE',  ( -0.000000000000000000, -0.000000000000000000, -1.000000000000000000 ) ) ;
#9485 = VERTEX_POINT ( 'NONE', #14824 ) ;
#9486 = FACE_OUTER_BOUND ( 'NONE', #23089, .T. ) ;
#9487 = ORIENTED_EDGE ( 'NONE', *, *, #10125, .F. ) ;
#9488 = CARTESIAN_POINT ( 'NONE',  ( -2.935661446561384391, -9.035036904804158553, -9.459589141758144137 ) ) ;
#9489 = VECTOR ( 'NONE', #12469, 1000.000000000000000 ) ;
#9490 = DIRECTION ( 'NONE',  ( 1.000000000000000000, 9.527085451588871562E-16, 0.000000000000000000 ) ) ;
#9491 = VECTOR ( 'NONE', #3228, 1000.000000000000000 ) ;
#9492 = EDGE_CURVE ( 'NONE', #17625, #18499, #18383, .T. ) ;
#9493 = ORIENTED_EDGE ( 'NONE', *, *, #22417, .F. ) ;
#9494 = EDGE_CURVE ( 'NONE', #15740, #4938, #12555, .T. ) ;
#9495 = LINE ( 'NONE', #262, #16133 ) ;
#9496 = DIRECTION ( 'NONE',  ( -0.000000000000000000, 1.000000000000000000, 1.224646799147353207E-16 ) ) ;
#9497 = AXIS2_PLACEMENT_3D ( 'NONE', #7532, #4385, #11797 ) ;
#9498 = CARTESIAN_POINT ( 'NONE',  ( 37.00000000000000711, -29.50000000000000355, 11.50000000000000000 ) ) ;
#9499 = FACE_OUTER_BOUND ( 'NONE', #19539, .T. ) ;
#9500 = CARTESIAN_POINT ( 'NONE',  ( 0.000000000000000000, -14.99147757894464306, 6.750000000000000888 ) ) ;
#9501 = CARTESIAN_POINT ( 'NONE',  ( 23.85000000000000497, 15.03999999999999915, -27.00000000000000000 ) ) ;
#9502 = VECTOR ( 'NONE', #13373, 1000.000000000000000 ) ;
#9503 = CARTESIAN_POINT ( 'NONE',  ( -2.935661446562617183, 9.035036904803758873, -6.659589141758144315 ) ) ;
#9504 = ORIENTED_EDGE ( 'NONE', *, *, #17306, .T. ) ;
#9505 = CIRCLE ( 'NONE', #16923, 5.000000000000007994 ) ;
#9506 = DIRECTION ( 'NONE',  ( 1.000000000000000000, 0.000000000000000000, -0.000000000000000000 ) ) ;
#9507 = EDGE_CURVE ( 'NONE', #4705, #7322, #9330, .T. ) ;
#9508 = ORIENTED_EDGE ( 'NONE', *, *, #6578, .T. ) ;
#9509 = DIRECTION ( 'NONE',  ( 0.000000000000000000, 0.000000000000000000, 1.000000000000000000 ) ) ;
#9510 = AXIS2_PLACEMENT_3D ( 'NONE', #21320, #13992, #1069 ) ;
#9511 = DIRECTION ( 'NONE',  ( 0.000000000000000000, 0.000000000000000000, 1.000000000000000000 ) ) ;
#9512 = CARTESIAN_POINT ( 'NONE',  ( -41.00000000000000000, -6.000000000000000888, 12.00000000000000000 ) ) ;
#9513 = CIRCLE ( 'NONE', #20438, 4.499999999999997335 ) ;
#9514 = CARTESIAN_POINT ( 'NONE',  ( 33.99999999999998579, -1.387778780781445676E-14, 10.49999999999999822 ) ) ;
#9515 = EDGE_CURVE ( 'NONE', #20283, #8446, #16774, .T. ) ;
#9516 = CARTESIAN_POINT ( 'NONE',  ( -20.85000000000000853, 15.04000000000000092, -25.00000000000000000 ) ) ;
#9517 = DIRECTION ( 'NONE',  ( 0.000000000000000000, 1.000000000000000000, 0.000000000000000000 ) ) ;
#9518 = DIRECTION ( 'NONE',  ( 0.000000000000000000, 0.000000000000000000, 1.000000000000000000 ) ) ;
#9519 = AXIS2_PLACEMENT_3D ( 'NONE', #14114, #12023, #23294 ) ;
#9520 = CARTESIAN_POINT ( 'NONE',  ( 73.42022815836234884, 7.420530141404717394E-15, 0.000000000000000000 ) ) ;
#9521 = VERTEX_POINT ( 'NONE', #20225 ) ;
#9522 = DIRECTION ( 'NONE',  ( 1.000000000000000000, 6.485355633664482599E-14, 0.000000000000000000 ) ) ;
#9523 = ADVANCED_FACE ( 'NONE', ( #1672 ), #20582, .T. ) ;
#9524 = CARTESIAN_POINT ( 'NONE',  ( 30.68762588338046982, -45.64284848299539732, -1.500000000000000000 ) ) ;
#9525 = EDGE_CURVE ( 'NONE', #13543, #3116, #22813, .T. ) ;
#9526 = CARTESIAN_POINT ( 'NONE',  ( 70.21613547800127719, 7.562528597612068045E-15, 0.000000000000000000 ) ) ;
#9527 = SHAPE_REPRESENTATION ( 'Housing Seal', ( #8005 ), #12698 ) ;
#9528 = DIRECTION ( 'NONE',  ( 1.000000000000000000, 0.000000000000000000, 0.000000000000000000 ) ) ;
#9529 = EDGE_LOOP ( 'NONE', ( #9940, #7652, #21287, #12968 ) ) ;
#9530 = VERTEX_POINT ( 'NONE', #22775 ) ;
#9531 = VECTOR ( 'NONE', #8447, 1000.000000000000000 ) ;
#9532 = VECTOR ( 'NONE', #11560, 1000.000000000000000 ) ;
#9533 = ORIENTED_EDGE ( 'NONE', *, *, #18146, .F. ) ;
#9534 = ORIENTED_EDGE ( 'NONE', *, *, #8088, .F. ) ;
#9535 = DIRECTION ( 'NONE',  ( 1.000000000000000000, 0.000000000000000000, 0.000000000000000000 ) ) ;
#9536 = VECTOR ( 'NONE', #12051, 1000.000000000000000 ) ;
#9537 = AXIS2_PLACEMENT_3D ( 'NONE', #18555, #3785, #1939 ) ;
#9538 = VECTOR ( 'NONE', #13634, 1000.000000000000000 ) ;
#9539 = CARTESIAN_POINT ( 'NONE',  ( -39.00000000000000000, 28.80990663662251805, 12.00000000000000000 ) ) ;
#9540 = ORIENTED_EDGE ( 'NONE', *, *, #5431, .F. ) ;
#9541 = ORIENTED_EDGE ( 'NONE', *, *, #22268, .F. ) ;
#9542 = ADVANCED_FACE ( 'NONE', ( #3976 ), #6059, .T. ) ;
#9543 = DIRECTION ( 'NONE',  ( -0.000000000000000000, -0.000000000000000000, -1.000000000000000000 ) ) ;
#9544 = ORIENTED_EDGE ( 'NONE', *, *, #2605, .F. ) ;
#9545 = CARTESIAN_POINT ( 'NONE',  ( -8.745930587506380860, -3.750307784154818247, -3.501341891226013914 ) ) ;
#9546 = ADVANCED_FACE ( 'NONE', ( #9800 ), #12937, .F. ) ;
#9547 = ORIENTED_EDGE ( 'NONE', *, *, #11607, .F. ) ;
#9548 = VECTOR ( 'NONE', #23166, 1000.000000000000000 ) ;
#9549 = CARTESIAN_POINT ( 'NONE',  ( -40.23082370883260239, 29.50000000000000711, -3.000000000000000000 ) ) ;
#9550 = CARTESIAN_POINT ( 'NONE',  ( 41.73082370883260239, 27.62204025492843940, -3.000000000000000000 ) ) ;
#9551 = CARTESIAN_POINT ( 'NONE',  ( 60.90909090909091361, 7.491529369508391930E-15, 0.000000000000000000 ) ) ;
#9552 = AXIS2_PLACEMENT_3D ( 'NONE', #23705, #6976, #1847 ) ;
#9553 = DIRECTION ( 'NONE',  ( 0.1313947906041688374, -0.9913301211009815095, 0.000000000000000000 ) ) ;
#9554 = ORIENTED_EDGE ( 'NONE', *, *, #5840, .T. ) ;
#9555 = PLANE ( 'NONE',  #14929 ) ;
#9556 = FACE_OUTER_BOUND ( 'NONE', #5473, .T. ) ;
#9557 = AXIS2_PLACEMENT_3D ( 'NONE', #14324, #14092, #2875 ) ;
#9558 = CIRCLE ( 'NONE', #5299, 20.85000000000000497 ) ;
#9559 = CARTESIAN_POINT ( 'NONE',  ( -7.022953521754877748, -5.102474405760673015, 5.833165578109188232 ) ) ;
#9560 = ORIENTED_EDGE ( 'NONE', *, *, #23289, .T. ) ;
#9561 = SHAPE_DEFINITION_REPRESENTATION ( #6522, #6130 ) ;
#9562 = ORIENTED_EDGE ( 'NONE', *, *, #19409, .F. ) ;
#9563 = ORIENTED_EDGE ( 'NONE', *, *, #19498, .F. ) ;
#9564 = FACE_OUTER_BOUND ( 'NONE', #11477, .T. ) ;
#9565 = CARTESIAN_POINT ( 'NONE',  ( 2.682529543900284974, -8.255977015246234174, -12.23316557810919036 ) ) ;
#9566 = CIRCLE ( 'NONE', #649, 4.249999999999996447 ) ;
#9567 = DIRECTION ( 'NONE',  ( -0.000000000000000000, -0.000000000000000000, -1.000000000000000000 ) ) ;
#9568 = AXIS2_PLACEMENT_3D ( 'NONE', #987, #8412, #15863 ) ;
#9569 = ORIENTED_EDGE ( 'NONE', *, *, #21368, .T. ) ;
#9570 = DIRECTION ( 'NONE',  ( -1.000000000000000000, 0.000000000000000000, 0.000000000000000000 ) ) ;
#9571 = CARTESIAN_POINT ( 'NONE',  ( 0.000000000000000000, 2.967071445749915881, 17.62702788437274393 ) ) ;
#9572 = CYLINDRICAL_SURFACE ( 'NONE', #21557, 11.00000000000000711 ) ;
#9573 = PRODUCT ( 'Assembly Drive shaft gear', 'Assembly Drive shaft gear', '', ( #3599 ) ) ;
#9574 = DIRECTION ( 'NONE',  ( -1.000000000000000000, -0.000000000000000000, -0.000000000000000000 ) ) ;
#9575 = LINE ( 'NONE', #22900, #17873 ) ;
#9576 = ORIENTED_EDGE ( 'NONE', *, *, #17301, .T. ) ;
#9577 = CARTESIAN_POINT ( 'NONE',  ( 80.69295543108962931, 6.123233995736675563E-16, -5.000000000000007994 ) ) ;
#9578 = CONICAL_SURFACE ( 'NONE', #1046, 10.50249999999999950, 0.7853981633974447263 ) ;
#9579 = CARTESIAN_POINT ( 'NONE',  ( -6.153822176767817416E-13, 9.500000000000000000, 3.499999999999999556 ) ) ;
#9580 = EDGE_CURVE ( 'NONE', #12142, #8729, #15676, .T. ) ;
#9581 = EDGE_CURVE ( 'NONE', #15077, #13001, #5170, .T. ) ;
#9582 = VERTEX_POINT ( 'NONE', #5925 ) ;
#9583 = CARTESIAN_POINT ( 'NONE',  ( -31.74999999999995737, 0.000000000000000000, 5.000000000000000888 ) ) ;
#9584 =( NAMED_UNIT ( * ) SI_UNIT ( $, .STERADIAN. ) SOLID_ANGLE_UNIT ( ) );
#9585 = CARTESIAN_POINT ( 'NONE',  ( -42.00000000000000711, 26.82133436441677077, 11.58578643762690241 ) ) ;
#9586 = PLANE ( 'NONE',  #14192 ) ;
#9587 = DIRECTION ( 'NONE',  ( -0.7071067811865469066, 0.000000000000000000, -0.7071067811865481278 ) ) ;
#9588 = CARTESIAN_POINT ( 'NONE',  ( 60.32931906745326245, 7.420530141404717394E-15, 0.000000000000000000 ) ) ;
#9589 = AXIS2_PLACEMENT_3D ( 'NONE', #16848, #16978, #6129 ) ;
#9590 = AXIS2_PLACEMENT_3D ( 'NONE', #19013, #4245, #17647 ) ;
#9591 = DIRECTION ( 'NONE',  ( 0.000000000000000000, 0.000000000000000000, 1.000000000000000000 ) ) ;
#9592 = ORIENTED_EDGE ( 'NONE', *, *, #4970, .F. ) ;
#9593 = VECTOR ( 'NONE', #1525, 1000.000000000000000 ) ;
#9594 = ORIENTED_EDGE ( 'NONE', *, *, #16620, .T. ) ;
#9595 = ORIENTED_EDGE ( 'NONE', *, *, #3511, .T. ) ;
#9596 = AXIS2_PLACEMENT_3D ( 'NONE', #18924, #11682, #8034 ) ;
#9597 = CARTESIAN_POINT ( 'NONE',  ( 5.871322893124551356, -8.081182679343980269, 9.759589141758143072 ) ) ;
#9598 = UNCERTAINTY_MEASURE_WITH_UNIT (LENGTH_MEASURE( 1.000000000000000082E-05 ), #20708, 'distance_accuracy_value', 'NONE');
#9599 = ADVANCED_FACE ( 'NONE', ( #11527 ), #2273, .T. ) ;
#9600 = DIRECTION ( 'NONE',  ( 0.000000000000000000, -1.224646799147353454E-16, 1.000000000000000000 ) ) ;
#9601 = CARTESIAN_POINT ( 'NONE',  ( -31.50000000000000711, -51.00000000000000711, 12.50000000000000000 ) ) ;
#9602 = DIRECTION ( 'NONE',  ( -0.000000000000000000, 0.000000000000000000, 1.000000000000000000 ) ) ;
#9603 = CIRCLE ( 'NONE', #22058, 5.000000000000007994 ) ;
#9604 = EDGE_CURVE ( 'NONE', #6728, #14555, #16088, .T. ) ;
#9605 = CYLINDRICAL_SURFACE ( 'NONE', #20356, 4.499999999999997335 ) ;
#9606 = EDGE_CURVE ( 'NONE', #3596, #17474, #11009, .T. ) ;
#9607 = CARTESIAN_POINT ( 'NONE',  ( 40.23082370883260239, 27.62204025492844650, -3.000000000000000000 ) ) ;
#9608 = EDGE_CURVE ( 'NONE', #23202, #3712, #21953, .T. ) ;
#9609 = CARTESIAN_POINT ( 'NONE',  ( -23.97499999999999787, -29.50000000000000000, -3.000000000000000000 ) ) ;
#9610 = DIRECTION ( 'NONE',  ( 1.000000000000000000, 0.000000000000000000, 0.000000000000000000 ) ) ;
#9611 = EDGE_CURVE ( 'NONE', #13451, #18900, #14904, .T. ) ;
#9612 = DIRECTION ( 'NONE',  ( -1.000000000000000000, 0.000000000000000000, 0.000000000000000000 ) ) ;
#9613 = DIRECTION ( 'NONE',  ( -1.000000000000000000, -0.000000000000000000, -0.000000000000000000 ) ) ;
#9614 = ORIENTED_EDGE ( 'NONE', *, *, #21199, .T. ) ;
#9615 = FACE_OUTER_BOUND ( 'NONE', #10535, .T. ) ;
#9616 = ORIENTED_EDGE ( 'NONE', *, *, #16616, .F. ) ;
#9617 = DIRECTION ( 'NONE',  ( -1.000000000000000000, 0.000000000000000000, 0.000000000000000000 ) ) ;
#9618 = ORIENTED_EDGE ( 'NONE', *, *, #20780, .T. ) ;
#9619 = CARTESIAN_POINT ( 'NONE',  ( 9.500000000000209610, -3.086737114211962396, 7.959589141758143249 ) ) ;
#9620 = ORIENTED_EDGE ( 'NONE', *, *, #23856, .F. ) ;
#9621 = DIRECTION ( 'NONE',  ( -0.000000000000000000, 0.000000000000000000, 1.000000000000000000 ) ) ;
#9622 = CARTESIAN_POINT ( 'NONE',  ( 5.000000000000000000, -3.513898075855363512, 2.028750000000008047 ) ) ;
#9623 = DIRECTION ( 'NONE',  ( -0.000000000000000000, -1.000000000000000000, -0.000000000000000000 ) ) ;
#9624 = EDGE_CURVE ( 'NONE', #22141, #15940, #11392, .T. ) ;
#9625 = CARTESIAN_POINT ( 'NONE',  ( 70.21613547800127719, 7.562528597612068045E-15, 0.000000000000000000 ) ) ;
#9626 = CARTESIAN_POINT ( 'NONE',  ( 69.05659179472598908, 6.123233995736675563E-16, -5.000000000000007994 ) ) ;
#9627 = AXIS2_PLACEMENT_3D ( 'NONE', #10274, #15400, #14065 ) ;
#9628 = EDGE_CURVE ( 'NONE', #21161, #16388, #13613, .T. ) ;
#9629 = CARTESIAN_POINT ( 'NONE',  ( -1.504652183083727168, 9.499999999999904077, -2.610843423304989308 ) ) ;
#9630 = VERTEX_POINT ( 'NONE', #4111 ) ;
#9631 = CARTESIAN_POINT ( 'NONE',  ( 2.935661446561383503, 9.035036904804158553, 11.60674201446023268 ) ) ;
#9632 = ADVANCED_FACE ( 'NONE', ( #329 ), #21055, .F. ) ;
#9633 = VERTEX_POINT ( 'NONE', #9579 ) ;
#9634 = CARTESIAN_POINT ( 'NONE',  ( 5.000000000000000000, 2.342598717236902939, -4.057500000000001883 ) ) ;
#9635 = CIRCLE ( 'NONE', #10803, 1.000000000000000888 ) ;
#9636 = CARTESIAN_POINT ( 'NONE',  ( 2.383518172110200339, 8.679382520702700887, 79.16775777249439727 ) ) ;
#9637 = CARTESIAN_POINT ( 'NONE',  ( 14.98950073861089294, 0.6491375924673389308, -9.483449329262333194 ) ) ;
#9638 = CYLINDRICAL_SURFACE ( 'NONE', #19075, 1.000000000000000000 ) ;
#9639 = CARTESIAN_POINT ( 'NONE',  ( -1.335344244249669021, 8.902285279863715317, 78.30632335935361255 ) ) ;
#9640 = DIRECTION ( 'NONE',  ( -0.000000000000000000, 1.000000000000000000, -0.000000000000000000 ) ) ;
#9641 = DIRECTION ( 'NONE',  ( 0.000000000000000000, -1.000000000000000000, 0.000000000000000000 ) ) ;
#9642 = CARTESIAN_POINT ( 'NONE',  ( 0.000000000000000000, 0.000000000000000000, 12.50000000000000000 ) ) ;
#9643 = ORIENTED_EDGE ( 'NONE', *, *, #1949, .F. ) ;
#9644 = FACE_OUTER_BOUND ( 'NONE', #6270, .T. ) ;
#9645 = CARTESIAN_POINT ( 'NONE',  ( 2.682529543900284974, -8.255977015246234174, 12.23316557810919036 ) ) ;
#9646 = CARTESIAN_POINT ( 'NONE',  ( -9.499999999999996447, 0.000000000000000000, 0.000000000000000000 ) ) ;
#9647 = DIRECTION ( 'NONE',  ( -1.000000000000000000, -1.224606353822377258E-16, -0.000000000000000000 ) ) ;
#9648 = AXIS2_PLACEMENT_3D ( 'NONE', #13364, #22773, #9689 ) ;
#9649 = EDGE_LOOP ( 'NONE', ( #14902, #15419, #7642, #20912, #21156, #1029 ) ) ;
#9650 = CONICAL_SURFACE ( 'NONE', #23725, 5.000000000000007994, 0.9599310885968855844 ) ;
#9651 = ITEM_DEFINED_TRANSFORMATION ( 'NONE', 'NONE', #15038,  #8005 ) ;
#9652 = ORIENTED_EDGE ( 'NONE', *, *, #22126, .F. ) ;
#9653 = FACE_OUTER_BOUND ( 'NONE', #18987, .T. ) ;
#9654 = CARTESIAN_POINT ( 'NONE',  ( 15.00000000000000355, 15.50000000000000000, 7.700000000000001954 ) ) ;
#9655 = ORIENTED_EDGE ( 'NONE', *, *, #20803, .T. ) ;
#9656 = AXIS2_PLACEMENT_3D ( 'NONE', #18697, #3927, #11596 ) ;
#9657 = ADVANCED_FACE ( 'NONE', ( #3860 ), #9442, .T. ) ;
#9658 = DIRECTION ( 'NONE',  ( -1.000000000000000000, 0.000000000000000000, -0.000000000000000000 ) ) ;
#9659 = VERTEX_POINT ( 'NONE', #22538 ) ;
#9660 = ORIENTED_EDGE ( 'NONE', *, *, #12749, .F. ) ;
#9661 = CARTESIAN_POINT ( 'NONE',  ( 71.96568270381689558, -5.000000000000009770, 0.000000000000000000 ) ) ;
#9662 = LINE ( 'NONE', #2615, #13328 ) ;
#9663 = FACE_OUTER_BOUND ( 'NONE', #4079, .T. ) ;
#9664 =( BOUNDED_CURVE ( )  B_SPLINE_CURVE ( 2, ( #3231, #21428, #5070, #18133, #6779, #12122, #12378, #15927, #12257, #12007, #10170 ),
 .UNSPECIFIED., .F., .T. ) 
 B_SPLINE_CURVE_WITH_KNOTS ( ( 3, 2, 2, 2, 2, 3 ),
 ( 0.4000000000000000222, 0.4199999999999999845, 0.4400000000000000022, 0.4599999999999999645, 0.4799999999999999267, 0.4999999999999999445 ),
 .UNSPECIFIED. ) 
 CURVE ( )  GEOMETRIC_REPRESENTATION_ITEM ( )  RATIONAL_B_SPLINE_CURVE ( ( 1.000000000000000000, 0.9510565162951535312, 1.000000000000000000, 0.9510565162951535312, 1.000000000000000000, 0.9510565162951535312, 1.000000000000000000, 0.9510565162951535312, 1.000000000000000000, 0.9510565162951536422, 0.9999999999999998890 ) ) 
 REPRESENTATION_ITEM ( '' )  );
#9665 = CARTESIAN_POINT ( 'NONE',  ( 4.489900896931573904, 0.000000000000000000, -8.500000000000000000 ) ) ;
#9666 = ORIENTED_EDGE ( 'NONE', *, *, #8709, .T. ) ;
#9667 = DIRECTION ( 'NONE',  ( -0.000000000000000000, -0.000000000000000000, -1.000000000000000000 ) ) ;
#9668 = CARTESIAN_POINT ( 'NONE',  ( -39.99999999999999289, 29.50000000000000000, 27.00000000000000000 ) ) ;
#9669 = CARTESIAN_POINT ( 'NONE',  ( -1.999999999999994449, -45.00000000000000000, 26.97499999999999432 ) ) ;
#9670 = VERTEX_POINT ( 'NONE', #15067 ) ;
#9671 = ORIENTED_EDGE ( 'NONE', *, *, #19883, .F. ) ;
#9672 = CARTESIAN_POINT ( 'NONE',  ( -7.022953521755574080, 5.102474405759713783, 3.433165578109189209 ) ) ;
#9673 = ORIENTED_EDGE ( 'NONE', *, *, #8197, .T. ) ;
#9674 = ORIENTED_EDGE ( 'NONE', *, *, #15659, .F. ) ;
#9675 = CLOSED_SHELL ( 'NONE', ( #13513, #6829, #2372, #6184, #13394, #21863, #21876, #13988, #12585, #21004, #11170, #5687, #12885, #23014, #4851, #22194, #22332, #687, #3198, #4402, #3507, #14692, #16761, #2662, #8847, #20241, #15429, #4312, #7817, #23066, #3509, #20712, #18412, #9232, #14302, #17821, #6994, #18284, #7084, #10399, #16006, #16606, #15736, #20307, #13817, #23808, #506, #17897, #9032, #4023, #7803, #3034, #73, #375, #16458, #20928, #11188, #11742, #15819, #7587, #13960, #1283, #22830, #19054, #14975, #15361, #3870, #16334, #22599, #3059, #7508, #18613, #9961, #6983, #2936, #4937, #1054, #991, #8569, #9632, #10523, #8563, #4366, #15186, #15734, #6909, #19730, #19978, #5894, #1357, #9546, #23671, #21857, #14575, #11536, #14884, #6787, #1259, #19367, #45, #15800, #11383, #20545, #15306, #13514, #9599, #5415, #3913, #22007, #13876, #9118, #22592, #11074, #15236, #527, #1106, #18404, #12452, #7879, #15004, #2041, #10362, #12292, #3757, #10985, #23668, #16281, #1560, #17866, #16330, #15823, #10126, #19370, #20617, #14035, #20231, #12755, #20158, #19128, #6602, #13309, #22297, #15264, #13789, #10278, #14478, #8402, #12814, #8795, #15951, #18916, #2161, #11687, #21293, #18328, #15358, #11316, #7471, #9523 ) ) ;
#9676 = EDGE_CURVE ( 'NONE', #6823, #12689, #14532, .T. ) ;
#9677 = CARTESIAN_POINT ( 'NONE',  ( 29.00000000000000000, -29.50000000000000355, 12.00000000000000000 ) ) ;
#9678 = ORIENTED_EDGE ( 'NONE', *, *, #8163, .F. ) ;
#9679 = ORIENTED_EDGE ( 'NONE', *, *, #5311, .T. ) ;
#9680 = ADVANCED_FACE ( 'NONE', ( #17028 ), #22645, .F. ) ;
#9681 = DIRECTION ( 'NONE',  ( 0.000000000000000000, -1.000000000000000000, 0.000000000000000000 ) ) ;
#9682 = DIRECTION ( 'NONE',  ( 0.000000000000000000, -0.000000000000000000, -1.000000000000000000 ) ) ;
#9683 = DIRECTION ( 'NONE',  ( -1.000000000000000000, -0.000000000000000000, -0.000000000000000000 ) ) ;
#9684 = ORIENTED_EDGE ( 'NONE', *, *, #23216, .F. ) ;
#9685 = DIRECTION ( 'NONE',  ( -0.000000000000000000, -0.000000000000000000, -1.000000000000000000 ) ) ;
#9686 = LINE ( 'NONE', #3970, #24012 ) ;
#9687 = LINE ( 'NONE', #7848, #22658 ) ;
#9688 = EDGE_CURVE ( 'NONE', #13092, #3902, #4605, .T. ) ;
#9689 = DIRECTION ( 'NONE',  ( -1.000000000000000000, 0.000000000000000000, 0.000000000000000000 ) ) ;
#9690 = ORIENTED_EDGE ( 'NONE', *, *, #6233, .F. ) ;
#9691 = DIRECTION ( 'NONE',  ( -0.000000000000000000, 0.000000000000000000, -1.000000000000000000 ) ) ;
#9692 = CARTESIAN_POINT ( 'NONE',  ( -31.74999999999995737, 0.000000000000000000, 0.000000000000000000 ) ) ;
#9693 = ORIENTED_EDGE ( 'NONE', *, *, #19958, .T. ) ;
#9694 = DIRECTION ( 'NONE',  ( 0.000000000000000000, 0.000000000000000000, 1.000000000000000000 ) ) ;
#9695 = DIRECTION ( 'NONE',  ( 0.000000000000000000, 1.000000000000000000, 0.000000000000000000 ) ) ;
#9696 = CARTESIAN_POINT ( 'NONE',  ( 17.15849686392983386, 8.309918483244988607, -4.628645577532790156 ) ) ;
#9697 = CARTESIAN_POINT ( 'NONE',  ( 58.00000000000000000, 7.491529369508391930E-15, 0.000000000000000000 ) ) ;
#9698 = CARTESIAN_POINT ( 'NONE',  ( 3.000000000000003109, 8.485281374238567764, 98.99999999999998579 ) ) ;
#9699 = SURFACE_SIDE_STYLE ('',( #2281 ) ) ;
#9700 = ORIENTED_EDGE ( 'NONE', *, *, #19184, .F. ) ;
#9701 = ORIENTED_EDGE ( 'NONE', *, *, #1149, .T. ) ;
#9702 = CARTESIAN_POINT ( 'NONE',  ( 5.365059087799946447, -7.384370330706356178, 10.33316557810919001 ) ) ;
#9703 = ORIENTED_EDGE ( 'NONE', *, *, #2089, .F. ) ;
#9704 = CARTESIAN_POINT ( 'NONE',  ( 40.00000000000000000, 28.80990663662251450, 11.00000000000000000 ) ) ;
#9705 = EDGE_CURVE ( 'NONE', #1921, #17955, #16487, .T. ) ;
#9706 = CARTESIAN_POINT ( 'NONE',  ( 0.000000000000000000, 14.21257171757157245, 0.08908218613057176938 ) ) ;
#9707 = EDGE_CURVE ( 'NONE', #5080, #6532, #19366, .T. ) ;
#9708 = AXIS2_PLACEMENT_3D ( 'NONE', #22168, #18497, #20320 ) ;
#9709 = AXIS2_PLACEMENT_3D ( 'NONE', #22936, #6094, #6209 ) ;
#9710 = CARTESIAN_POINT ( 'NONE',  ( 5.998136232247472499, -6.550536670409162987, 12.49999999999999289 ) ) ;
#9711 = LINE ( 'NONE', #13142, #16636 ) ;
#9712 = CARTESIAN_POINT ( 'NONE',  ( -33.24999999999999289, -29.50000000000000000, -2.224999999999995204 ) ) ;
#9713 = LINE ( 'NONE', #4710, #11372 ) ;
#9714 = VERTEX_POINT ( 'NONE', #6662 ) ;
#9715 = ORIENTED_EDGE ( 'NONE', *, *, #3843, .F. ) ;
#9716 = CARTESIAN_POINT ( 'NONE',  ( 73.42022815836234884, 7.420530141404717394E-15, 0.000000000000000000 ) ) ;
#9717 = CARTESIAN_POINT ( 'NONE',  ( 0.000000000000000000, 0.000000000000000000, 12.00000000000000000 ) ) ;
#9718 = CARTESIAN_POINT ( 'NONE',  ( 41.99999999999999289, 25.93535998569253920, 27.00000000000000000 ) ) ;
#9719 = FACE_OUTER_BOUND ( 'NONE', #12894, .T. ) ;
#9720 = DIRECTION ( 'NONE',  ( 1.000000000000000000, 0.000000000000000000, 0.000000000000000000 ) ) ;
#9721 = ORIENTED_EDGE ( 'NONE', *, *, #7213, .F. ) ;
#9722 = EDGE_CURVE ( 'NONE', #7449, #3425, #11088, .T. ) ;
#9723 = ORIENTED_EDGE ( 'NONE', *, *, #22586, .F. ) ;
#9724 = CIRCLE ( 'NONE', #8161, 4.499999999999997335 ) ;
#9725 = DIRECTION ( 'NONE',  ( 2.600433232233976523E-16, -1.000000000000000000, 0.000000000000000000 ) ) ;
#9726 = VERTEX_POINT ( 'NONE', #17508 ) ;
#9727 = EDGE_CURVE ( 'NONE', #14353, #13648, #23506, .T. ) ;
#9728 = DIRECTION ( 'NONE',  ( 0.000000000000000000, -1.000000000000000000, 4.625929269271485322E-15 ) ) ;
#9729 = CARTESIAN_POINT ( 'NONE',  ( -36.00000000000001421, 50.99999999999999289, 0.000000000000000000 ) ) ;
#9730 = EDGE_CURVE ( 'NONE', #18077, #15534, #10245, .T. ) ;
#9731 = CARTESIAN_POINT ( 'NONE',  ( 33.99999999999998579, 4.999999999999985789, 9.500000000000000000 ) ) ;
#9732 = EDGE_CURVE ( 'NONE', #16017, #21225, #11893, .T. ) ;
#9733 = DIRECTION ( 'NONE',  ( 1.000000000000000000, 0.000000000000000000, 0.000000000000000000 ) ) ;
#9734 = DIRECTION ( 'NONE',  ( 0.000000000000000000, -1.000000000000000000, 0.000000000000000000 ) ) ;
#9735 = LINE ( 'NONE', #17193, #10201 ) ;
#9736 = ORIENTED_EDGE ( 'NONE', *, *, #4161, .T. ) ;
#9737 = CIRCLE ( 'NONE', #11283, 11.23082370883259706 ) ;
#9738 = DIRECTION ( 'NONE',  ( 1.000000000000000000, 0.000000000000000000, -0.000000000000000000 ) ) ;
#9739 = ORIENTED_EDGE ( 'NONE', *, *, #236, .F. ) ;
#9740 = DIRECTION ( 'NONE',  ( -1.000000000000000000, -0.000000000000000000, -0.000000000000000000 ) ) ;
#9741 = FACE_OUTER_BOUND ( 'NONE', #12390, .T. ) ;
#9742 = CARTESIAN_POINT ( 'NONE',  ( 60.03431729618309021, -1.232595164407830946E-29, 5.000000000000007994 ) ) ;
#9743 = DIRECTION ( 'NONE',  ( 0.000000000000000000, 0.000000000000000000, -1.000000000000000000 ) ) ;
#9744 = CARTESIAN_POINT ( 'NONE',  ( 0.000000000000000000, 12.00453763395397466, 7.608955687739546114 ) ) ;
#9745 = CARTESIAN_POINT ( 'NONE',  ( 11.50000000000000000, 17.02535186363803632, 5.445458559199172655 ) ) ;
#9746 = CARTESIAN_POINT ( 'NONE',  ( 42.00000000000000000, -6.000000000000015099, 11.00000000000000000 ) ) ;
#9747 = EDGE_CURVE ( 'NONE', #3762, #21057, #18448, .T. ) ;
#9748 = CARTESIAN_POINT ( 'NONE',  ( -7.685661446562381371, 5.583959896777970222, -6.006742014460233037 ) ) ;
#9749 = ORIENTED_EDGE ( 'NONE', *, *, #16187, .T. ) ;
#9750 = LINE ( 'NONE', #4558, #3911 ) ;
#9751 = CARTESIAN_POINT ( 'NONE',  ( 7.022953521755574080, -5.102474405759714671, 10.43316557810918788 ) ) ;
#9752 = DIRECTION ( 'NONE',  ( 0.000000000000000000, 1.000000000000000000, 0.000000000000000000 ) ) ;
#9753 = DIRECTION ( 'NONE',  ( -1.000000000000000000, 0.000000000000000000, 0.000000000000000000 ) ) ;
#9754 = DIRECTION ( 'NONE',  ( -1.000000000000000000, 0.000000000000000000, 0.000000000000000000 ) ) ;
#9755 = AXIS2_PLACEMENT_3D ( 'NONE', #1688, #1468, #5583 ) ;
#9756 = EDGE_CURVE ( 'NONE', #22991, #13688, #2448, .T. ) ;
#9757 = EDGE_CURVE ( 'NONE', #15653, #16665, #4416, .T. ) ;
#9758 = EDGE_CURVE ( 'NONE', #6894, #12373, #6780, .T. ) ;
#9759 = CIRCLE ( 'NONE', #4743, 1.000000000000000888 ) ;
#9760 = ORIENTED_EDGE ( 'NONE', *, *, #2396, .F. ) ;
#9761 = CARTESIAN_POINT ( 'NONE',  ( 57.42022815836235594, 7.420530141404717394E-15, 0.000000000000000000 ) ) ;
#9762 = CARTESIAN_POINT ( 'NONE',  ( -9.500000000000211386, 3.086737114211961064, -10.10674201446023446 ) ) ;
#9763 = VERTEX_POINT ( 'NONE', #10429 ) ;
#9764 = CARTESIAN_POINT ( 'NONE',  ( -37.00000000000000711, -29.49999999999999645, 12.00000000000000000 ) ) ;
#9765 = ORIENTED_EDGE ( 'NONE', *, *, #622, .T. ) ;
#9766 = CYLINDRICAL_SURFACE ( 'NONE', #2658, 8.000000000000000000 ) ;
#9767 = VECTOR ( 'NONE', #3408, 1000.000000000000000 ) ;
#9768 = VERTEX_POINT ( 'NONE', #21548 ) ;
#9769 = DIRECTION ( 'NONE',  ( 0.000000000000000000, 0.000000000000000000, 1.000000000000000000 ) ) ;
#9770 = DIRECTION ( 'NONE',  ( -0.000000000000000000, 0.000000000000000000, 1.000000000000000000 ) ) ;
#9771 = CIRCLE ( 'NONE', #5916, 5.000000000000007994 ) ;
#9772 = DIRECTION ( 'NONE',  ( 1.000000000000000000, 0.000000000000000000, 0.000000000000000000 ) ) ;
#9773 = DIRECTION ( 'NONE',  ( -0.5000000000000003331, 0.8660254037844384856, 0.000000000000000000 ) ) ;
#9774 = ORIENTED_EDGE ( 'NONE', *, *, #7832, .T. ) ;
#9775 = FACE_OUTER_BOUND ( 'NONE', #19055, .T. ) ;
#9776 = DIRECTION ( 'NONE',  ( -1.000000000000000000, 0.000000000000000000, 0.000000000000000000 ) ) ;
#9777 = EDGE_LOOP ( 'NONE', ( #1621, #14430, #18857, #21412 ) ) ;
#9778 = ORIENTED_EDGE ( 'NONE', *, *, #3577, .T. ) ;
#9779 = CARTESIAN_POINT ( 'NONE',  ( -7.685661446561619314, -5.583959896779019161, 11.25958914175814307 ) ) ;
#9780 = ORIENTED_EDGE ( 'NONE', *, *, #17214, .T. ) ;
#9781 = ORIENTED_EDGE ( 'NONE', *, *, #21946, .T. ) ;
#9782 = ADVANCED_FACE ( 'NONE', ( #19729 ), #2859, .F. ) ;
#9783 = DIRECTION ( 'NONE',  ( -0.000000000000000000, -0.000000000000000000, -1.000000000000000000 ) ) ;
#9784 = ADVANCED_FACE ( 'NONE', ( #8483 ), #6906, .F. ) ;
#9785 = CIRCLE ( 'NONE', #22275, 18.50000000000000000 ) ;
#9786 = EDGE_LOOP ( 'NONE', ( #2694, #19894, #16434, #3897 ) ) ;
#9787 = EDGE_LOOP ( 'NONE', ( #8869, #23549, #16562, #21326 ) ) ;
#9788 = CIRCLE ( 'NONE', #16050, 1.999999999999994449 ) ;
#9789 = AXIS2_PLACEMENT_3D ( 'NONE', #9991, #14150, #15979 ) ;
#9790 = DIRECTION ( 'NONE',  ( -0.000000000000000000, -0.000000000000000000, -1.000000000000000000 ) ) ;
#9791 = CARTESIAN_POINT ( 'NONE',  ( -5.365059087799947335, 7.384370330706355290, -3.333165578109187344 ) ) ;
#9792 = TOROIDAL_SURFACE ( 'NONE', #22677, 10.94716442891539643, 0.2999999999999999334 ) ;
#9793 = DIRECTION ( 'NONE',  ( 1.000000000000000000, 0.000000000000000000, 0.000000000000000000 ) ) ;
#9794 = EDGE_LOOP ( 'NONE', ( #21601, #18384, #19274, #4128 ) ) ;
#9795 = FACE_OUTER_BOUND ( 'NONE', #15839, .T. ) ;
#9796 = FACE_OUTER_BOUND ( 'NONE', #21455, .T. ) ;
#9797 = DIRECTION ( 'NONE',  ( -1.000000000000000000, 0.000000000000000000, 0.000000000000000000 ) ) ;
#9798 = ORIENTED_EDGE ( 'NONE', *, *, #20184, .T. ) ;
#9799 = CYLINDRICAL_SURFACE ( 'NONE', #4134, 5.000000000000000888 ) ;
#9800 = FACE_OUTER_BOUND ( 'NONE', #5667, .T. ) ;
#9801 = EDGE_CURVE ( 'NONE', #7244, #20252, #10308, .T. ) ;
#9802 = ORIENTED_EDGE ( 'NONE', *, *, #398, .T. ) ;
#9803 = CARTESIAN_POINT ( 'NONE',  ( 23.85000000000000497, 15.03999999999999915, 25.00000000000000000 ) ) ;
#9804 = FACE_OUTER_BOUND ( 'NONE', #3441, .T. ) ;
#9805 = CARTESIAN_POINT ( 'NONE',  ( -20.64923905428956630, -37.45138642374539728, 11.00000000000000000 ) ) ;
#9806 = AXIS2_PLACEMENT_3D ( 'NONE', #4259, #19025, #11424 ) ;
#9807 = CARTESIAN_POINT ( 'NONE',  ( -9.500000000000000000, -6.482511860946779655E-13, -5.059589141758143782 ) ) ;
#9808 = EDGE_CURVE ( 'NONE', #12373, #2607, #5973, .T. ) ;
#9809 = CARTESIAN_POINT ( 'NONE',  ( 7.022953521754877748, 5.102474405760673903, -10.83316557810919001 ) ) ;
#9810 = CIRCLE ( 'NONE', #19964, 51.49999999999999289 ) ;
#9811 = CIRCLE ( 'NONE', #14869, 5.000000000000007994 ) ;
#9812 = CARTESIAN_POINT ( 'NONE',  ( 7.685661446562381371, -5.583959896777971110, -9.006742014460233037 ) ) ;
#9813 = CIRCLE ( 'NONE', #14889, 10.02592346138681201 ) ;
#9814 = CIRCLE ( 'NONE', #2843, 18.50000000000000000 ) ;
#9815 = EDGE_LOOP ( 'NONE', ( #7809, #15992, #8086, #8698 ) ) ;
#9816 = ORIENTED_EDGE ( 'NONE', *, *, #9425, .F. ) ;
#9817 = AXIS2_PLACEMENT_3D ( 'NONE', #21526, #4828, #2989 ) ;
#9818 = ADVANCED_FACE ( 'NONE', ( #4482 ), #20080, .F. ) ;
#9819 = CARTESIAN_POINT ( 'NONE',  ( -2.682529543899159208, -8.255977015246598327, 12.03316557810918930 ) ) ;
#9820 = VECTOR ( 'NONE', #3796, 1000.000000000000000 ) ;
#9821 = EDGE_LOOP ( 'NONE', ( #23874, #11508, #21753, #11938 ) ) ;
#9822 = CARTESIAN_POINT ( 'NONE',  ( 28.79496467126520542, 30.58653375045326683, 48.72831690717703168 ) ) ;
#9823 = DIRECTION ( 'NONE',  ( 0.000000000000000000, -1.000000000000000000, 0.000000000000000000 ) ) ;
#9824 = ORIENTED_EDGE ( 'NONE', *, *, #2941, .F. ) ;
#9825 = CARTESIAN_POINT ( 'NONE',  ( -20.99999999999999645, 29.49999999999999645, 12.00000000000000000 ) ) ;
#9826 = PRODUCT_DEFINITION_CONTEXT ( 'detailed design', #4014, 'design' ) ;
#9827 = CARTESIAN_POINT ( 'NONE',  ( 0.000000000000000000, 0.000000000000000000, -3.000000000000000000 ) ) ;
#9829 = AXIS2_PLACEMENT_3D ( 'NONE', #8718, #807, #15671 ) ;
#9828 = CARTESIAN_POINT ( 'NONE',  ( -42.00000000000000000, 5.000000000000000888, 11.00000000000000000 ) ) ;
#9830 = FACE_OUTER_BOUND ( 'NONE', #14834, .T. ) ;
#9831 = ORIENTED_EDGE ( 'NONE', *, *, #166, .F. ) ;
#9832 = AXIS2_PLACEMENT_3D ( 'NONE', #12799, #10946, #18419 ) ;
#9833 = VERTEX_POINT ( 'NONE', #18798 ) ;
#9834 = DIRECTION ( 'NONE',  ( 0.7052211081716895924, 0.7089874389501509278, -0.000000000000000000 ) ) ;
#9835 = AXIS2_PLACEMENT_3D ( 'NONE', #22784, #18878, #1809 ) ;
#9836 = CYLINDRICAL_SURFACE ( 'NONE', #3576, 17.25000000000000000 ) ;
#9837 = CIRCLE ( 'NONE', #18810, 1.500000000000001332 ) ;
#9838 = FACE_OUTER_BOUND ( 'NONE', #4804, .T. ) ;
#9839 = EDGE_CURVE ( 'NONE', #14009, #4646, #13064, .T. ) ;
#9840 = ORIENTED_EDGE ( 'NONE', *, *, #8709, .F. ) ;
#9841 = DIRECTION ( 'NONE',  ( -0.000000000000000000, -0.000000000000000000, -1.000000000000000000 ) ) ;
#9842 = CARTESIAN_POINT ( 'NONE',  ( -41.73082370883260239, 27.62204025492845361, -3.000000000000000000 ) ) ;
#9843 = CIRCLE ( 'NONE', #11404, 17.25000000000000000 ) ;
#9844 = LINE ( 'NONE', #8518, #20391 ) ;
#9845 = CARTESIAN_POINT ( 'NONE',  ( -5.871322893123449127, -8.081182679344781405, 4.506742014460232149 ) ) ;
#9846 = EDGE_CURVE ( 'NONE', #3762, #9763, #22339, .T. ) ;
#9847 = ORIENTED_EDGE ( 'NONE', *, *, #14057, .F. ) ;
#9848 = ORIENTED_EDGE ( 'NONE', *, *, #16363, .F. ) ;
#9849 = ORIENTED_EDGE ( 'NONE', *, *, #23310, .T. ) ;
#9850 = AXIS2_PLACEMENT_3D ( 'NONE', #14387, #14042, #23567 ) ;
#9851 = CARTESIAN_POINT ( 'NONE',  ( -7.685661446561619314, -5.583959896779019161, 11.25958914175814307 ) ) ;
#9852 = CARTESIAN_POINT ( 'NONE',  ( 9.500000000000000000, 6.470877716354879437E-13, 13.20674201446023410 ) ) ;
#9853 = AXIS2_PLACEMENT_3D ( 'NONE', #19871, #16205, #18036 ) ;
#9854 = CIRCLE ( 'NONE', #938, 4.249999999999996447 ) ;
#9855 = ORIENTED_EDGE ( 'NONE', *, *, #17756, .T. ) ;
#9856 = CIRCLE ( 'NONE', #16113, 2.500000000000002220 ) ;
#9857 = ADVANCED_BREP_SHAPE_REPRESENTATION ( '', ( #2277, #8005 ), #9178 ) ;
#9858 = CARTESIAN_POINT ( 'NONE',  ( 73.42022815836234884, 6.123233995736675563E-16, -5.000000000000007994 ) ) ;
#9859 = AXIS2_PLACEMENT_3D ( 'NONE', #5064, #18127, #3908 ) ;
#9860 = PLANE ( 'NONE',  #15438 ) ;
#9861 = ORIENTED_EDGE ( 'NONE', *, *, #1188, .T. ) ;
#9862 = VECTOR ( 'NONE', #7717, 999.9999999999998863 ) ;
#9863 = LINE ( 'NONE', #8036, #22818 ) ;
#9864 = VECTOR ( 'NONE', #18541, 1000.000000000000000 ) ;
#9865 = CARTESIAN_POINT ( 'NONE',  ( 7.751944208201828168, -4.001916517787142524, -12.50000000000000178 ) ) ;
#9866 = DIRECTION ( 'NONE',  ( -1.000000000000000000, 0.000000000000000000, 0.000000000000000000 ) ) ;
#9867 = CARTESIAN_POINT ( 'NONE',  ( -9.500000000000000000, -6.482511860946779655E-13, -3.059589141758143338 ) ) ;
#9868 = EDGE_LOOP ( 'NONE', ( #21534, #22282, #10547, #15978, #6622, #5699 ) ) ;
#9869 = CARTESIAN_POINT ( 'NONE',  ( 0.000000000000000000, -15.23000000000000220, 27.00000000000000000 ) ) ;
#9870 = ORIENTED_EDGE ( 'NONE', *, *, #23492, .F. ) ;
#9871 = CARTESIAN_POINT ( 'NONE',  ( 3.934052222107095265, -8.094642247421083070, 12.50000000000000000 ) ) ;
#9872 = DIRECTION ( 'NONE',  ( 0.000000000000000000, 0.000000000000000000, 1.000000000000000000 ) ) ;
#9873 = CARTESIAN_POINT ( 'NONE',  ( 74.87477361290781630, 5.000000000000007105, 6.123233995736765296E-16 ) ) ;
#9874 = CIRCLE ( 'NONE', #13004, 8.000000000000003553 ) ;
#9875 = CARTESIAN_POINT ( 'NONE',  ( 87.67068093254673045, -1.078520768856852078E-29, 5.000000000000007994 ) ) ;
#9876 = EDGE_CURVE ( 'NONE', #11779, #23352, #21157, .T. ) ;
#9877 = CIRCLE ( 'NONE', #14178, 4.999999999999997335 ) ;
#9878 = CARTESIAN_POINT ( 'NONE',  ( 75.45454545454545325, 4.172000000000015696, 5.109226446042767468E-16 ) ) ;
#9879 = EDGE_CURVE ( 'NONE', #17662, #9290, #13292, .T. ) ;
#9880 = VECTOR ( 'NONE', #8746, 1000.000000000000000 ) ;
#9881 = DIRECTION ( 'NONE',  ( -0.000000000000000000, -0.000000000000000000, -1.000000000000000000 ) ) ;
#9882 = DIRECTION ( 'NONE',  ( -1.000000000000000000, -1.224606353822377258E-16, -0.000000000000000000 ) ) ;
#9883 = ORIENTED_EDGE ( 'NONE', *, *, #23015, .T. ) ;
#9884 = CARTESIAN_POINT ( 'NONE',  ( -1.504652183083727168, 9.499999999999904077, -3.757996296007079184 ) ) ;
#9885 = CIRCLE ( 'NONE', #2895, 1.000000000000000888 ) ;
#9886 = EDGE_LOOP ( 'NONE', ( #3968, #13226, #533, #18415, #20911 ) ) ;
#9887 = CARTESIAN_POINT ( 'NONE',  ( 0.000000000000000000, 8.890849273385601492, 7.584660931657517757 ) ) ;
#9888 = CARTESIAN_POINT ( 'NONE',  ( 5.365059087798939252, 7.384370330707087149, 10.93316557810918965 ) ) ;
#9889 = DIRECTION ( 'NONE',  ( -1.000000000000000000, -0.000000000000000000, -0.000000000000000000 ) ) ;
#9890 = CARTESIAN_POINT ( 'NONE',  ( -41.73082370883258108, -27.62204025492845716, -1.500000000000000000 ) ) ;
#9891 = AXIS2_PLACEMENT_3D ( 'NONE', #12910, #20371, #16454 ) ;
#9892 = AXIS2_PLACEMENT_3D ( 'NONE', #5389, #10614, #18208 ) ;
#9893 = B_SPLINE_CURVE_WITH_KNOTS ( 'NONE', 3,
 ( #6416, #13860, #8476, #17390, #10300, #17882, #11997, #19469 ),
 .UNSPECIFIED., .F., .F.,
 ( 4, 2, 2, 4 ),
 ( 1.734723475976807094E-18, 0.001946159586596642828, 0.002919239379894964133, 0.003892319173193285655 ),
 .UNSPECIFIED. ) ;
#9894 = ORIENTED_EDGE ( 'NONE', *, *, #16439, .T. ) ;
#9895 = DIRECTION ( 'NONE',  ( -0.000000000000000000, -0.000000000000000000, -1.000000000000000000 ) ) ;
#9896 = CIRCLE ( 'NONE', #13024, 5.000000000000007994 ) ;
#9897 = EDGE_CURVE ( 'NONE', #17902, #4215, #22582, .T. ) ;
#9898 = CARTESIAN_POINT ( 'NONE',  ( 5.871322893123449127, 8.081182679344781405, -11.50674201446023126 ) ) ;
#9899 = ORIENTED_EDGE ( 'NONE', *, *, #9507, .T. ) ;
#9900 = CIRCLE ( 'NONE', #15755, 20.85000000000000142 ) ;
#9901 = SPHERICAL_SURFACE ( 'NONE', #12759, 1.500000000000000000 ) ;
#9902 = ORIENTED_EDGE ( 'NONE', *, *, #16147, .T. ) ;
#9903 = FACE_OUTER_BOUND ( 'NONE', #2370, .T. ) ;
#9904 = EDGE_CURVE ( 'NONE', #10554, #20510, #16248, .T. ) ;
#9905 = EDGE_CURVE ( 'NONE', #14771, #581, #9073, .T. ) ;
#9906 = ORIENTED_EDGE ( 'NONE', *, *, #11291, .T. ) ;
#9907 = EDGE_CURVE ( 'NONE', #14363, #5776, #1426, .T. ) ;
#9908 = CARTESIAN_POINT ( 'NONE',  ( 61.78386452199871570, 7.420530141404717394E-15, 0.000000000000000000 ) ) ;
#9909 = DIRECTION ( 'NONE',  ( -0.5654966663575777819, -0.8247505806839220410, 0.000000000000000000 ) ) ;
#9910 = DIRECTION ( 'NONE',  ( 1.000000000000000000, 0.000000000000000000, 0.000000000000000000 ) ) ;
#9911 = CIRCLE ( 'NONE', #585, 1.500000000000001332 ) ;
#9912 = AXIS2_PLACEMENT_3D ( 'NONE', #22218, #12917, #11434 ) ;
#9913 = DIRECTION ( 'NONE',  ( 0.5735764363510424957, 0.8191520442889943521, 0.000000000000000000 ) ) ;
#9914 = ORIENTED_EDGE ( 'NONE', *, *, #11607, .T. ) ;
#9915 = CARTESIAN_POINT ( 'NONE',  ( -12.50000000000000178, 1.672973214995343413E-15, 2.500000000000000000 ) ) ;
#9916 = DIRECTION ( 'NONE',  ( -1.000000000000000000, -0.000000000000000000, -0.000000000000000000 ) ) ;
#9917 = DIRECTION ( 'NONE',  ( 0.000000000000000000, 0.000000000000000000, -1.000000000000000000 ) ) ;
#9918 = ORIENTED_EDGE ( 'NONE', *, *, #9897, .T. ) ;
#9919 = AXIS2_PLACEMENT_3D ( 'NONE', #2278, #16913, #7749 ) ;
#9920 = ORIENTED_EDGE ( 'NONE', *, *, #8118, .T. ) ;
#9921 = CARTESIAN_POINT ( 'NONE',  ( 5.871322893123449127, 8.081182679344781405, 10.35958914175814627 ) ) ;
#9922 = ORIENTED_EDGE ( 'NONE', *, *, #8220, .T. ) ;
#9923 = ORIENTED_EDGE ( 'NONE', *, *, #23850, .F. ) ;
#9924 = AXIS2_PLACEMENT_3D ( 'NONE', #12634, #21324, #1550 ) ;
#9925 = VERTEX_POINT ( 'NONE', #2080 ) ;
#9926 = VERTEX_POINT ( 'NONE', #23742 ) ;
#9927 = DIRECTION ( 'NONE',  ( -0.000000000000000000, -0.000000000000000000, -1.000000000000000000 ) ) ;
#9928 = CARTESIAN_POINT ( 'NONE',  ( -2.682529543899159208, -8.255977015246598327, -4.033165578109189298 ) ) ;
#9929 = CARTESIAN_POINT ( 'NONE',  ( 58.87477361290780919, 7.420530141404717394E-15, 0.000000000000000000 ) ) ;
#9930 = EDGE_CURVE ( 'NONE', #22874, #17607, #9443, .T. ) ;
#9931 = ORIENTED_EDGE ( 'NONE', *, *, #3154, .T. ) ;
#9932 = CARTESIAN_POINT ( 'NONE',  ( 5.000000000000000000, 0.000000000000000000, 0.000000000000000000 ) ) ;
#9933 = CARTESIAN_POINT ( 'NONE',  ( -6.250000000000000888, 10.82531754730548279, -2.500000000000000000 ) ) ;
#9934 = CARTESIAN_POINT ( 'NONE',  ( -31.74999999999995737, 6.123233995736767268E-16, -5.000000000000000888 ) ) ;
#9935 = LINE ( 'NONE', #931, #16333 ) ;
#9936 = VECTOR ( 'NONE', #16513, 1000.000000000000114 ) ;
#9937 = ORIENTED_EDGE ( 'NONE', *, *, #9325, .T. ) ;
#9938 = CARTESIAN_POINT ( 'NONE',  ( -9.500000000000000000, -6.482511860946779655E-13, -6.206742014460234103 ) ) ;
#9939 = VECTOR ( 'NONE', #5982, 1000.000000000000000 ) ;
#9940 = ORIENTED_EDGE ( 'NONE', *, *, #3191, .T. ) ;
#9941 = LINE ( 'NONE', #17403, #10876 ) ;
#9942 = EDGE_CURVE ( 'NONE', #19249, #20685, #6762, .T. ) ;
#9943 = CARTESIAN_POINT ( 'NONE',  ( 0.000000000000000000, -3.205857990849823480, 11.23818298448541420 ) ) ;
#9944 = FACE_OUTER_BOUND ( 'NONE', #16457, .T. ) ;
#9945 = CARTESIAN_POINT ( 'NONE',  ( 7.022953521754877748, 5.102474405760673903, -8.833165578109190008 ) ) ;
#9946 = VERTEX_POINT ( 'NONE', #13175 ) ;
#9947 = ORIENTED_EDGE ( 'NONE', *, *, #4288, .F. ) ;
#9948 = CIRCLE ( 'NONE', #13488, 4.172000000000008590 ) ;
#9949 = ORIENTED_EDGE ( 'NONE', *, *, #17350, .F. ) ;
#9950 = DIRECTION ( 'NONE',  ( -8.773087109899882274E-17, 5.449134320520223463E-16, -1.000000000000000000 ) ) ;
#9951 = FACE_OUTER_BOUND ( 'NONE', #4242, .T. ) ;
#9952 = VECTOR ( 'NONE', #11548, 1000.000000000000000 ) ;
#9953 = ORIENTED_EDGE ( 'NONE', *, *, #20484, .T. ) ;
#9954 = DIRECTION ( 'NONE',  ( 0.000000000000000000, 0.000000000000000000, 1.000000000000000000 ) ) ;
#9955 = CIRCLE ( 'NONE', #5704, 5.000000000000007994 ) ;
#9956 = VECTOR ( 'NONE', #7136, 1000.000000000000000 ) ;
#9957 = CIRCLE ( 'NONE', #1799, 23.84999999999999432 ) ;
#9958 = CARTESIAN_POINT ( 'NONE',  ( -31.74999999999995737, 0.000000000000000000, 0.000000000000000000 ) ) ;
#9959 = DIRECTION ( 'NONE',  ( 4.613626265895764052E-16, 1.000000000000000000, 0.000000000000000000 ) ) ;
#9960 = CARTESIAN_POINT ( 'NONE',  ( 40.66734255040738333, 26.56420859267091217, -3.000000000000000000 ) ) ;
#9961 = ADVANCED_FACE ( 'NONE', ( #20632, #12614 ), #11456, .T. ) ;
#9962 = ORIENTED_EDGE ( 'NONE', *, *, #23067, .T. ) ;
#9963 = CARTESIAN_POINT ( 'NONE',  ( 78.19113660963670043, 9.032993985154128325, 0.000000000000000000 ) ) ;
#9964 = CARTESIAN_POINT ( 'NONE',  ( 5.000000000000000000, -4.685197434473820088, 9.540979117872439019E-15 ) ) ;
#9965 = EDGE_CURVE ( 'NONE', #1786, #4017, #11320, .T. ) ;
#9966 = CYLINDRICAL_SURFACE ( 'NONE', #13433, 9.500000000000000000 ) ;
#9967 = DIRECTION ( 'NONE',  ( 0.000000000000000000, 1.000000000000000000, 0.000000000000000000 ) ) ;
#9968 = EDGE_CURVE ( 'NONE', #19120, #18612, #12196, .T. ) ;
#9969 = CARTESIAN_POINT ( 'NONE',  ( 37.00000000000000711, -29.50000000000000355, 12.00000000000000000 ) ) ;
#9970 = CARTESIAN_POINT ( 'NONE',  ( 23.00000000000000000, 5.823083658124882156, -12.96521604808343398 ) ) ;
#9971 = PRODUCT_DEFINITION_FORMATION_WITH_SPECIFIED_SOURCE ( 'ANY', '', #21328, .NOT_KNOWN. ) ;
#9972 = LINE ( 'NONE', #2919, #3671 ) ;
#9973 = ORIENTED_EDGE ( 'NONE', *, *, #22003, .F. ) ;
#9974 = ORIENTED_EDGE ( 'NONE', *, *, #21500, .F. ) ;
#9975 = CARTESIAN_POINT ( 'NONE',  ( 9.500000000000209610, -3.086737114211962396, 11.95958914175814591 ) ) ;
#9976 = CARTESIAN_POINT ( 'NONE',  ( 2.935661446561383503, 9.035036904804158553, 11.60674201446023268 ) ) ;
#9977 = ORIENTED_EDGE ( 'NONE', *, *, #20017, .F. ) ;
#9978 = LINE ( 'NONE', #2800, #17702 ) ;
#9979 = CARTESIAN_POINT ( 'NONE',  ( 12.50000000000000178, 5.755434930044642846E-15, 2.500000000000000000 ) ) ;
#9980 = CARTESIAN_POINT ( 'NONE',  ( 61.48886275072855057, 7.562528597612068045E-15, 0.000000000000000000 ) ) ;
#9981 = EDGE_CURVE ( 'NONE', #9714, #19452, #14325, .T. ) ;
#9982 = TOROIDAL_SURFACE ( 'NONE', #1458, 19.84999999999999787, 1.000000000000000000 ) ;
#9983 = DIRECTION ( 'NONE',  ( 0.000000000000000000, 0.000000000000000000, 1.000000000000000000 ) ) ;
#9984 = CARTESIAN_POINT ( 'NONE',  ( 0.000000000000000000, 0.000000000000000000, 0.000000000000000000 ) ) ;
#9985 = DIRECTION ( 'NONE',  ( -1.000000000000000000, -1.224606353822377258E-16, -0.000000000000000000 ) ) ;
#9986 = CARTESIAN_POINT ( 'NONE',  ( 61.78386452199871570, 5.000000000000016875, 6.123233995736777129E-16 ) ) ;
#9987 = EDGE_CURVE ( 'NONE', #22195, #1759, #3357, .T. ) ;
#9989 = EDGE_CURVE ( 'NONE', #21516, #2764, #22701, .T. ) ;
#9988 = CARTESIAN_POINT ( 'NONE',  ( -2.935661446562617183, 9.035036904803758873, -2.659589141758143871 ) ) ;
#9990 = ORIENTED_EDGE ( 'NONE', *, *, #20851, .T. ) ;
#9991 = CARTESIAN_POINT ( 'NONE',  ( 0.000000000000000000, -45.00000000000000000, 0.02500000000000418554 ) ) ;
#9992 = ADVANCED_FACE ( 'NONE', ( #864 ), #8159, .F. ) ;
#9993 = VERTEX_POINT ( 'NONE', #4546 ) ;
#9994 = DIRECTION ( 'NONE',  ( 1.000000000000000000, 0.000000000000000000, 0.000000000000000000 ) ) ;
#9995 = CARTESIAN_POINT ( 'NONE',  ( 41.73082370883258818, -27.62204025492844650, -1.500000000000000000 ) ) ;
#9996 = CARTESIAN_POINT ( 'NONE',  ( -29.00000000000000000, -29.49999999999999645, 11.50000000000000000 ) ) ;
#9997 = DIRECTION ( 'NONE',  ( 1.000000000000000000, 1.224606353822377258E-16, 0.000000000000000000 ) ) ;
#9998 = CARTESIAN_POINT ( 'NONE',  ( -21.13207267780287069, -38.32709852940855910, 11.00000000000000000 ) ) ;
#9999 = ORIENTED_EDGE ( 'NONE', *, *, #10999, .F. ) ;
#10000 = CARTESIAN_POINT ( 'NONE',  ( 9.500000000000000000, 6.470877716354879437E-13, -7.206742014460234103 ) ) ;
#10001 = CARTESIAN_POINT ( 'NONE',  ( 5.871322893123448239, 8.081182679344781405, 8.359589141758144493 ) ) ;
#10002 = EDGE_LOOP ( 'NONE', ( #21485, #16788, #16631, #14505 ) ) ;
#10003 = CARTESIAN_POINT ( 'NONE',  ( -5.871322893124554021, 8.081182679343978492, -7.906742014460233392 ) ) ;
#10004 = ORIENTED_EDGE ( 'NONE', *, *, #6798, .T. ) ;
#10005 = DIRECTION ( 'NONE',  ( -0.000000000000000000, -0.000000000000000000, -1.000000000000000000 ) ) ;
#10006 = CARTESIAN_POINT ( 'NONE',  ( -8.680847955710813579, -2.820578480814257549, 7.733165578109188587 ) ) ;
#10007 = LINE ( 'NONE', #23455, #8436 ) ;
#10008 = PRODUCT_DEFINITION ( 'UNKNOWN', '', #3373, #9826 ) ;
#10009 = CARTESIAN_POINT ( 'NONE',  ( -33.24999999999999289, 29.50000000000000000, -2.224999999999995204 ) ) ;
#10010 = ADVANCED_FACE ( 'NONE', ( #17331 ), #13928, .F. ) ;
#10011 = VERTEX_POINT ( 'NONE', #749 ) ;
#10012 = ADVANCED_FACE ( 'NONE', ( #13670 ), #6487, .T. ) ;
#10013 = EDGE_LOOP ( 'NONE', ( #9289, #14679, #9848, #15474 ) ) ;
#10014 = LINE ( 'NONE', #8180, #16621 ) ;
#10015 = EDGE_CURVE ( 'NONE', #19090, #12662, #10262, .T. ) ;
#10016 = CARTESIAN_POINT ( 'NONE',  ( 9.500000000000209610, -3.086737114211962396, -11.10674201446023446 ) ) ;
#10017 = EDGE_LOOP ( 'NONE', ( #20237, #13082, #21053, #17586 ) ) ;
#10018 = ORIENTED_EDGE ( 'NONE', *, *, #8381, .F. ) ;
#10019 = LINE ( 'NONE', #4810, #23312 ) ;
#10020 = ORIENTED_EDGE ( 'NONE', *, *, #12294, .T. ) ;
#10021 = ORIENTED_EDGE ( 'NONE', *, *, #1836, .F. ) ;
#10022 = DIRECTION ( 'NONE',  ( 0.000000000000000000, -0.5406408174555868973, -0.8412535328311879779 ) ) ;
#10023 = DIRECTION ( 'NONE',  ( 1.000000000000000000, 0.000000000000000000, 0.000000000000000000 ) ) ;
#10024 = FACE_OUTER_BOUND ( 'NONE', #12418, .T. ) ;
#10025 = CARTESIAN_POINT ( 'NONE',  ( -28.00000000000001066, 50.99999999999999289, 0.5000000000000000000 ) ) ;
#10026 = ORIENTED_EDGE ( 'NONE', *, *, #19026, .F. ) ;
#10027 = DIRECTION ( 'NONE',  ( 1.000000000000000000, 0.000000000000000000, 0.000000000000000000 ) ) ;
#10028 = DIRECTION ( 'NONE',  ( -1.000000000000000000, -0.000000000000000000, -0.000000000000000000 ) ) ;
#10029 = DIRECTION ( 'NONE',  ( 0.000000000000000000, -1.000000000000000000, 0.000000000000000000 ) ) ;
#10030 = ORIENTED_EDGE ( 'NONE', *, *, #8432, .T. ) ;
#10031 = PRODUCT_RELATED_PRODUCT_CATEGORY ( 'part', '', ( #13924 ) ) ;
#10032 = AXIS2_PLACEMENT_3D ( 'NONE', #14461, #22287, #18025 ) ;
#10033 = ORIENTED_EDGE ( 'NONE', *, *, #4941, .F. ) ;
#10034 = CARTESIAN_POINT ( 'NONE',  ( 6.809999908187194197E-13, -9.988891130263535700, 9.559589141758145558 ) ) ;
#10035 = EDGE_CURVE ( 'NONE', #17416, #3007, #19165, .T. ) ;
#10036 = ORIENTED_EDGE ( 'NONE', *, *, #19546, .T. ) ;
#10037 = ORIENTED_EDGE ( 'NONE', *, *, #20288, .F. ) ;
#10038 = ORIENTED_EDGE ( 'NONE', *, *, #12883, .T. ) ;
#10039 = EDGE_CURVE ( 'NONE', #8700, #20652, #18072, .T. ) ;
#10040 = ORIENTED_EDGE ( 'NONE', *, *, #14351, .T. ) ;
#10041 = ADVANCED_FACE ( 'NONE', ( #22842, #19295 ), #19534, .F. ) ;
#10042 = CARTESIAN_POINT ( 'NONE',  ( 0.000000000000000000, 10.59264252385236915, 4.936618945406632264 ) ) ;
#10043 = FACE_OUTER_BOUND ( 'NONE', #13967, .T. ) ;
#10044 = EDGE_CURVE ( 'NONE', #3733, #22670, #17753, .T. ) ;
#10045 = CARTESIAN_POINT ( 'NONE',  ( 5.871322893123448239, 8.081182679344781405, 7.506742014460233037 ) ) ;
#10046 = VERTEX_POINT ( 'NONE', #7790 ) ;
#10047 = CARTESIAN_POINT ( 'NONE',  ( -14.51962751333974389, 3.765689428759031010, -27.00000000000000000 ) ) ;
#10048 = CARTESIAN_POINT ( 'NONE',  ( -31.74999999999995737, 0.000000000000000000, 5.000000000000000888 ) ) ;
#10049 = CARTESIAN_POINT ( 'NONE',  ( -31.74999999999995737, 0.000000000000000000, 0.000000000000000000 ) ) ;
#10050 = CARTESIAN_POINT ( 'NONE',  ( -31.74999999999995737, 6.123233995736767268E-16, -5.000000000000000888 ) ) ;
#10051 = DIRECTION ( 'NONE',  ( -0.000000000000000000, -0.000000000000000000, 1.000000000000000000 ) ) ;
#10052 = ORIENTED_EDGE ( 'NONE', *, *, #10621, .F. ) ;
#10053 = CIRCLE ( 'NONE', #23337, 9.500000000000000000 ) ;
#10054 = DIRECTION ( 'NONE',  ( 0.000000000000000000, -1.000000000000000000, 0.000000000000000000 ) ) ;
#10055 = ORIENTED_EDGE ( 'NONE', *, *, #17628, .T. ) ;
#10056 = DIRECTION ( 'NONE',  ( -1.000000000000000000, 0.000000000000000000, 0.000000000000000000 ) ) ;
#10057 = CARTESIAN_POINT ( 'NONE',  ( 40.23082370883260239, 27.62204025492844650, -1.500000000000000000 ) ) ;
#10058 = DIRECTION ( 'NONE',  ( 0.000000000000000000, 0.000000000000000000, -1.000000000000000000 ) ) ;
#10059 = CARTESIAN_POINT ( 'NONE',  ( 28.99999999999999645, 29.49999999999999645, -3.000000000000000000 ) ) ;
#10060 = CARTESIAN_POINT ( 'NONE',  ( 5.365059087798939252, 7.384370330707087149, -8.933165578109187877 ) ) ;
#10061 = CIRCLE ( 'NONE', #15936, 6.050000000006050982 ) ;
#10062 = EDGE_LOOP ( 'NONE', ( #8302, #21040, #22829 ) ) ;
#10063 = CARTESIAN_POINT ( 'NONE',  ( 39.00000000000000000, -29.49999999999999645, 12.00000000000000000 ) ) ;
#10064 = ORIENTED_EDGE ( 'NONE', *, *, #10395, .F. ) ;
#10065 = ADVANCED_FACE ( 'NONE', ( #11694 ), #14919, .T. ) ;
#10066 = ORIENTED_EDGE ( 'NONE', *, *, #20336, .F. ) ;
#10067 = CARTESIAN_POINT ( 'NONE',  ( 7.022953521755574080, -5.102474405759714671, 8.433165578109187877 ) ) ;
#10068 = VERTEX_POINT ( 'NONE', #21965 ) ;
#10069 = AXIS2_PLACEMENT_3D ( 'NONE', #17836, #6489, #10111 ) ;
#10070 = DIRECTION ( 'NONE',  ( -0.000000000000000000, -0.000000000000000000, -1.000000000000000000 ) ) ;
#10071 = EDGE_LOOP ( 'NONE', ( #2650, #3877, #8182, #8583 ) ) ;
#10072 = ADVANCED_FACE ( 'NONE', ( #19895, #18196 ), #14276, .T. ) ;
#10073 = DIRECTION ( 'NONE',  ( 0.000000000000000000, -1.000000000000000000, 0.000000000000000000 ) ) ;
#10074 = CARTESIAN_POINT ( 'NONE',  ( 5.000000000000000000, -2.342598717236905603, 4.057500000000010765 ) ) ;
#10075 = UNCERTAINTY_MEASURE_WITH_UNIT (LENGTH_MEASURE( 1.000000000000000082E-05 ), #19890, 'distance_accuracy_value', 'NONE');
#10076 = EDGE_CURVE ( 'NONE', #1617, #23304, #6376, .T. ) ;
#10077 = DIRECTION ( 'NONE',  ( -1.000000000000000000, -0.000000000000000000, -0.000000000000000000 ) ) ;
#10078 = DIRECTION ( 'NONE',  ( 1.000000000000000000, 0.000000000000000000, 0.000000000000000000 ) ) ;
#10079 = DIRECTION ( 'NONE',  ( -1.000000000000000000, -0.000000000000000000, 0.000000000000000000 ) ) ;
#10080 = VECTOR ( 'NONE', #17526, 1000.000000000000000 ) ;
#10081 = EDGE_LOOP ( 'NONE', ( #3634, #720, #683, #23950 ) ) ;
#10082 = CARTESIAN_POINT ( 'NONE',  ( 0.000000000000000000, 0.000000000000000000, 0.4999999999999970024 ) ) ;
#10083 = DIRECTION ( 'NONE',  ( 0.000000000000000000, 0.000000000000000000, -1.000000000000000000 ) ) ;
#10084 = DIRECTION ( 'NONE',  ( 0.000000000000000000, -1.000000000000000000, 0.000000000000000000 ) ) ;
#10085 = FACE_OUTER_BOUND ( 'NONE', #21775, .T. ) ;
#10086 = CARTESIAN_POINT ( 'NONE',  ( 0.3000000000000023204, 1.191082103573950144E-15, -9.725923461386809521 ) ) ;
#10087 =( REPRESENTATION_RELATIONSHIP ('NONE','NONE', #21748, #15960 ) REPRESENTATION_RELATIONSHIP_WITH_TRANSFORMATION ( #655 )SHAPE_REPRESENTATION_RELATIONSHIP( ) );
#10088 = DIRECTION ( 'NONE',  ( 1.000000000000000000, -0.000000000000000000, 0.000000000000000000 ) ) ;
#10089 = CIRCLE ( 'NONE', #6173, 9.499999999999996447 ) ;
#10090 = EDGE_LOOP ( 'NONE', ( #4784, #11819, #22824, #21038 ) ) ;
#10091 = CARTESIAN_POINT ( 'NONE',  ( -9.500000000000000000, -6.482511860946779655E-13, -12.20674201446023410 ) ) ;
#10092 = ORIENTED_EDGE ( 'NONE', *, *, #817, .F. ) ;
#10093 = EDGE_LOOP ( 'NONE', ( #11716, #8797, #16270, #22681 ) ) ;
#10094 = CARTESIAN_POINT ( 'NONE',  ( -2.935661446562617183, 9.035036904803758873, 10.65958914175814343 ) ) ;
#10095 = CARTESIAN_POINT ( 'NONE',  ( -9.500000000000211386, 3.086737114211961064, 12.10674201446023091 ) ) ;
#10096 = VERTEX_POINT ( 'NONE', #21736 ) ;
#10097 = AXIS2_PLACEMENT_3D ( 'NONE', #3601, #23988, #1784 ) ;
#10098 = CARTESIAN_POINT ( 'NONE',  ( 70.51113724927145654, 7.420530141404717394E-15, 0.000000000000000000 ) ) ;
#10099 = LINE ( 'NONE', #19780, #13453 ) ;
#10100 = DIRECTION ( 'NONE',  ( -0.000000000000000000, -0.000000000000000000, -1.000000000000000000 ) ) ;
#10101 = EDGE_CURVE ( 'NONE', #9181, #21814, #7064, .T. ) ;
#10102 = CARTESIAN_POINT ( 'NONE',  ( 34.02500000000000568, -29.50000000000000000, -3.000000000000000000 ) ) ;
#10103 = CYLINDRICAL_SURFACE ( 'NONE', #2192, 9.000000000000000000 ) ;
#10104 = CARTESIAN_POINT ( 'NONE',  ( 90.00000000000000000, 0.000000000000000000, 0.000000000000000000 ) ) ;
#10105 = FACE_BOUND ( 'NONE', #23257, .T. ) ;
#10106 = ORIENTED_EDGE ( 'NONE', *, *, #21028, .F. ) ;
#10107 = ORIENTED_EDGE ( 'NONE', *, *, #18189, .F. ) ;
#10108 = DIRECTION ( 'NONE',  ( -0.000000000000000000, -0.000000000000000000, -1.000000000000000000 ) ) ;
#10109 = CARTESIAN_POINT ( 'NONE',  ( -41.73082370883260239, 29.50000000000000711, -1.500000000000000000 ) ) ;
#10110 = LINE ( 'NONE', #11826, #5956 ) ;
#10111 = DIRECTION ( 'NONE',  ( 0.000000000000000000, 1.000000000000000000, 0.000000000000000000 ) ) ;
#10112 = CIRCLE ( 'NONE', #19886, 49.99999999999999289 ) ;
#10113 = CARTESIAN_POINT ( 'NONE',  ( 35.99999999999999289, -51.00000000000000711, 12.50000000000000000 ) ) ;
#10114 = ORIENTED_EDGE ( 'NONE', *, *, #5847, .T. ) ;
#10115 = ADVANCED_FACE ( 'NONE', ( #16232, #3169 ), #15874, .F. ) ;
#10116 = CARTESIAN_POINT ( 'NONE',  ( 40.49999999999998579, 50.99999999999999289, 0.5000000000000004441 ) ) ;
#10117 = LINE ( 'NONE', #4554, #6454 ) ;
#10118 = ORIENTED_EDGE ( 'NONE', *, *, #9727, .T. ) ;
#10119 = CARTESIAN_POINT ( 'NONE',  ( -2.935661446562617183, 9.035036904803758873, -7.806742014460233747 ) ) ;
#10120 = ORIENTED_EDGE ( 'NONE', *, *, #22449, .T. ) ;
#10121 = DIRECTION ( 'NONE',  ( -1.000000000000000000, 0.000000000000000000, 0.000000000000000000 ) ) ;
#10122 = EDGE_CURVE ( 'NONE', #4241, #555, #17677, .T. ) ;
#10123 = CARTESIAN_POINT ( 'NONE',  ( -8.680847955711200825, 2.820578480813073607, 9.533165578109189298 ) ) ;
#10124 = FACE_OUTER_BOUND ( 'NONE', #17840, .T. ) ;
#10125 = EDGE_CURVE ( 'NONE', #13543, #11621, #8423, .T. ) ;
#10126 = ADVANCED_FACE ( 'NONE', ( #1363 ), #18841, .T. ) ;
#10127 = ORIENTED_EDGE ( 'NONE', *, *, #20075, .F. ) ;
#10129 = VERTEX_POINT ( 'NONE', #3065 ) ;
#10128 = CIRCLE ( 'NONE', #19112, 5.000000000000007994 ) ;
#10130 = ORIENTED_EDGE ( 'NONE', *, *, #20817, .T. ) ;
#10131 = CARTESIAN_POINT ( 'NONE',  ( 40.00000000000000711, 15.50000000000000533, 19.70000000000000284 ) ) ;
#10132 = CARTESIAN_POINT ( 'NONE',  ( 6.809999908187194197E-13, -9.988891130263535700, -12.70674201446023410 ) ) ;
#10133 = VERTEX_POINT ( 'NONE', #12433 ) ;
#10134 = EDGE_LOOP ( 'NONE', ( #21887, #15593, #20262, #822 ) ) ;
#10135 = CARTESIAN_POINT ( 'NONE',  ( 69.05659179472598908, 7.420530141404717394E-15, 0.000000000000000000 ) ) ;
#10136 = LINE ( 'NONE', #2141, #9101 ) ;
#10137 = ORIENTED_EDGE ( 'NONE', *, *, #11843, .F. ) ;
#10138 = FACE_OUTER_BOUND ( 'NONE', #14453, .T. ) ;
#10139 = ORIENTED_EDGE ( 'NONE', *, *, #3707, .F. ) ;
#10140 = DIRECTION ( 'NONE',  ( 0.000000000000000000, -1.000000000000000000, 0.000000000000000000 ) ) ;
#10141 = LINE ( 'NONE', #18970, #23861 ) ;
#10142 = CARTESIAN_POINT ( 'NONE',  ( 0.3000000000000020983, 0.000000000000000000, 0.000000000000000000 ) ) ;
#10143 = DIRECTION ( 'NONE',  ( 0.000000000000000000, 0.000000000000000000, 1.000000000000000000 ) ) ;
#10144 = CONICAL_SURFACE ( 'NONE', #7047, 4.172000000000008590, 0.9599310885968742602 ) ;
#10145 = ORIENTED_EDGE ( 'NONE', *, *, #13320, .T. ) ;
#10146 = LINE ( 'NONE', #23112, #20413 ) ;
#10147 = EDGE_CURVE ( 'NONE', #18900, #20705, #19671, .T. ) ;
#10148 = LINE ( 'NONE', #21036, #1325 ) ;
#10149 = EDGE_CURVE ( 'NONE', #9099, #18771, #2206, .T. ) ;
#10150 = CARTESIAN_POINT ( 'NONE',  ( 0.000000000000000000, 0.000000000000000000, -27.00000000000000000 ) ) ;
#10151 = ORIENTED_EDGE ( 'NONE', *, *, #18283, .F. ) ;
#10152 = VERTEX_POINT ( 'NONE', #21487 ) ;
#10153 = CARTESIAN_POINT ( 'NONE',  ( -9.499999999999790390, -3.086737114213257804, 9.159589141758145203 ) ) ;
#10154 = ORIENTED_EDGE ( 'NONE', *, *, #2761, .F. ) ;
#10155 = MANIFOLD_SOLID_BREP ( 'Mirror3', #7726 ) ;
#10156 = ORIENTED_EDGE ( 'NONE', *, *, #14171, .T. ) ;
#10157 = ORIENTED_EDGE ( 'NONE', *, *, #15449, .F. ) ;
#10158 = FACE_BOUND ( 'NONE', #11293, .T. ) ;
#10159 = CARTESIAN_POINT ( 'NONE',  ( 2.682529543900284974, -8.255977015246234174, -4.233165578109187699 ) ) ;
#10160 = DIRECTION ( 'NONE',  ( -1.000000000000000000, 0.000000000000000000, 0.000000000000000000 ) ) ;
#10161 = CARTESIAN_POINT ( 'NONE',  ( -9.500000000000000000, -6.482511860946779655E-13, -6.206742014460234103 ) ) ;
#10162 = CIRCLE ( 'NONE', #9370, 5.000000000000007994 ) ;
#10163 = ORIENTED_EDGE ( 'NONE', *, *, #16375, .T. ) ;
#10164 = CARTESIAN_POINT ( 'NONE',  ( -16.36913330654531507, -6.602951766536811817, -6.845624079409802221 ) ) ;
#10165 = CARTESIAN_POINT ( 'NONE',  ( 9.499999999999996447, 1.163414459189985091E-15, 0.000000000000000000 ) ) ;
#10166 = CYLINDRICAL_SURFACE ( 'NONE', #10992, 1.000000000000000888 ) ;
#10167 = DIRECTION ( 'NONE',  ( -0.000000000000000000, -0.000000000000000000, -1.000000000000000000 ) ) ;
#10168 = CIRCLE ( 'NONE', #11710, 0.9999999999999994449 ) ;
#10169 = ORIENTED_EDGE ( 'NONE', *, *, #20077, .F. ) ;
#10170 = CARTESIAN_POINT ( 'NONE',  ( -9.500000000000000000, -6.482511860946779655E-13, -8.206742014460234103 ) ) ;
#10171 = DIRECTION ( 'NONE',  ( -1.000000000000000000, 0.000000000000000000, 0.000000000000000000 ) ) ;
#10172 = VERTEX_POINT ( 'NONE', #997 ) ;
#10173 = CARTESIAN_POINT ( 'NONE',  ( -23.84999999999999432, -15.03999999999999915, 25.00000000000000000 ) ) ;
#10174 = DIRECTION ( 'NONE',  ( 0.000000000000000000, 0.000000000000000000, 1.000000000000000000 ) ) ;
#10175 = CARTESIAN_POINT ( 'NONE',  ( 17.57797814737053699, -9.461914562436907872, -0.9781177603712922775 ) ) ;
#10176 = CARTESIAN_POINT ( 'NONE',  ( -28.99999999999999645, -29.50000000000001066, 27.00000000000000000 ) ) ;
#10177 = EDGE_CURVE ( 'NONE', #22995, #3150, #23918, .T. ) ;
#10178 = CARTESIAN_POINT ( 'NONE',  ( 8.680847955710813579, 2.820578480814259326, -8.733165578109186811 ) ) ;
#10179 = EDGE_CURVE ( 'NONE', #12687, #14244, #3779, .T. ) ;
#10180 = CARTESIAN_POINT ( 'NONE',  ( 74.00000000000001421, 7.491529369508391930E-15, 0.000000000000000000 ) ) ;
#10181 = VERTEX_POINT ( 'NONE', #3532 ) ;
#10182 = ORIENTED_EDGE ( 'NONE', *, *, #5668, .F. ) ;
#10183 = AXIS2_PLACEMENT_3D ( 'NONE', #4010, #471, #11427 ) ;
#10184 = CARTESIAN_POINT ( 'NONE',  ( -8.680847955711007202, -5.923547351154968927E-13, -11.63316557810919072 ) ) ;
#10185 = CARTESIAN_POINT ( 'NONE',  ( 2.682529543899157876, 8.255977015246598327, 11.03316557810918752 ) ) ;
#10186 = PRODUCT ( 'Nipple', 'Nipple', '', ( #23754 ) ) ;
#10187 = AXIS2_PLACEMENT_3D ( 'NONE', #2119, #4203, #15267 ) ;
#10188 = ORIENTED_EDGE ( 'NONE', *, *, #10035, .F. ) ;
#10189 = DIRECTION ( 'NONE',  ( 0.000000000000000000, 0.000000000000000000, 1.000000000000000000 ) ) ;
#10190 = LINE ( 'NONE', #11654, #1133 ) ;
#10191 = ORIENTED_EDGE ( 'NONE', *, *, #22860, .T. ) ;
#10192 = CARTESIAN_POINT ( 'NONE',  ( -18.50000000000000000, 15.23000000000000220, -27.00000000000000000 ) ) ;
#10193 = DIRECTION ( 'NONE',  ( 1.000000000000000000, 1.224606353822377258E-16, 0.000000000000000000 ) ) ;
#10194 = DIRECTION ( 'NONE',  ( 1.000000000000000000, 0.000000000000000000, 0.000000000000000000 ) ) ;
#10195 = DIRECTION ( 'NONE',  ( 0.000000000000000000, 1.000000000000000000, 0.000000000000000000 ) ) ;
#10196 = ORIENTED_EDGE ( 'NONE', *, *, #13323, .F. ) ;
#10197 = DIRECTION ( 'NONE',  ( -0.000000000000000000, -0.000000000000000000, -1.000000000000000000 ) ) ;
#10198 = DIRECTION ( 'NONE',  ( -1.000000000000000000, 0.000000000000000000, 0.000000000000000000 ) ) ;
#10199 = EDGE_CURVE ( 'NONE', #8089, #3297, #14635, .T. ) ;
#10200 = CIRCLE ( 'NONE', #13317, 18.50000000000000000 ) ;
#10201 = VECTOR ( 'NONE', #19290, 1000.000000000000000 ) ;
#10202 = AXIS2_PLACEMENT_3D ( 'NONE', #19914, #12564, #23704 ) ;
#10203 = LINE ( 'NONE', #17665, #15354 ) ;
#10204 = ORIENTED_EDGE ( 'NONE', *, *, #5629, .T. ) ;
#10205 = FACE_OUTER_BOUND ( 'NONE', #4289, .T. ) ;
#10206 = CARTESIAN_POINT ( 'NONE',  ( 0.000000000000000000, 45.00000000000000000, -27.00000000000000000 ) ) ;
#10207 = CARTESIAN_POINT ( 'NONE',  ( -27.89784171216405895, -41.49349862090491570, -1.500000000000000000 ) ) ;
#10208 = AXIS2_PLACEMENT_3D ( 'NONE', #2486, #15520, #9909 ) ;
#10209 = TOROIDAL_SURFACE ( 'NONE', #12543, 2.500000000000001776, 1.000000000000000000 ) ;
#10210 = DIRECTION ( 'NONE',  ( 1.000000000000000000, 0.000000000000000000, 0.000000000000000000 ) ) ;
#10211 = EDGE_CURVE ( 'NONE', #8434, #977, #250, .T. ) ;
#10212 = VERTEX_POINT ( 'NONE', #5610 ) ;
#10213 = CARTESIAN_POINT ( 'NONE',  ( 7.685661446561619314, 5.583959896779020049, -11.40674201446023517 ) ) ;
#10214 = ADVANCED_FACE ( 'NONE', ( #1832 ), #9134, .F. ) ;
#10215 = EDGE_LOOP ( 'NONE', ( #3347, #6216, #11048, #3276 ) ) ;
#10216 = VERTEX_POINT ( 'NONE', #20493 ) ;
#10217 = CARTESIAN_POINT ( 'NONE',  ( 2.935661446561383503, 9.035036904804158553, 4.459589141758144137 ) ) ;
#10218 = CARTESIAN_POINT ( 'NONE',  ( 6.809999908187194197E-13, -9.988891130263535700, 10.70674201446023233 ) ) ;
#10219 = EDGE_LOOP ( 'NONE', ( #7238, #11230 ) ) ;
#10220 =( LENGTH_UNIT ( ) NAMED_UNIT ( * ) SI_UNIT ( .MILLI., .METRE. ) );
#10221 = DIRECTION ( 'NONE',  ( -0.8247505806839219300, -0.5654966663575777819, 2.861428388275804004E-15 ) ) ;
#10222 = CARTESIAN_POINT ( 'NONE',  ( 0.000000000000000000, 0.000000000000000000, -3.499999999999999556 ) ) ;
#10223 = AXIS2_PLACEMENT_3D ( 'NONE', #16672, #12644, #5567 ) ;
#10224 = AXIS2_PLACEMENT_3D ( 'NONE', #20624, #18780, #5855 ) ;
#10225 = VECTOR ( 'NONE', #15985, 1000.000000000000000 ) ;
#10226 = CARTESIAN_POINT ( 'NONE',  ( -0.9830802669677229932, 45.00000000000000000, 0.000000000000000000 ) ) ;
#10227 = DIRECTION ( 'NONE',  ( -1.000000000000000000, -1.224606353822377258E-16, -0.000000000000000000 ) ) ;
#10228 = AXIS2_PLACEMENT_3D ( 'NONE', #22088, #5360, #16567 ) ;
#10229 = AXIS2_PLACEMENT_3D ( 'NONE', #12673, #16444, #23912 ) ;
#10230 = VECTOR ( 'NONE', #5102, 1000.000000000000000 ) ;
#10231 = CIRCLE ( 'NONE', #18039, 51.49999999999999289 ) ;
#10232 = DIRECTION ( 'NONE',  ( -0.000000000000000000, 0.000000000000000000, -1.000000000000000000 ) ) ;
#10233 = LINE ( 'NONE', #4654, #21540 ) ;
#10234 = AXIS2_PLACEMENT_3D ( 'NONE', #18322, #8206, #1386 ) ;
#10235 = ADVANCED_FACE ( 'NONE', ( #20256 ), #16452, .F. ) ;
#10236 = VERTEX_POINT ( 'NONE', #14749 ) ;
#10237 = CARTESIAN_POINT ( 'NONE',  ( 41.73082370883257397, -29.49999999999999645, -1.500000000000000000 ) ) ;
#10238 = APPLICATION_CONTEXT ( 'automotive_design' ) ;
#10239 = EDGE_LOOP ( 'NONE', ( #20505, #8288, #17383, #4732 ) ) ;
#10240 = DIRECTION ( 'NONE',  ( -1.000000000000000000, 0.000000000000000000, 0.000000000000000000 ) ) ;
#10241 = CARTESIAN_POINT ( 'NONE',  ( -6.232140916353180238, -6.843256600934770617, 12.27698021605092471 ) ) ;
#10242 = CARTESIAN_POINT ( 'NONE',  ( 6.809999908187194197E-13, -9.988891130263535700, 11.55958914175814201 ) ) ;
#10243 = DIRECTION ( 'NONE',  ( 0.000000000000000000, -0.000000000000000000, 1.000000000000000000 ) ) ;
#10244 = EDGE_CURVE ( 'NONE', #1409, #9993, #20796, .T. ) ;
#10245 = CIRCLE ( 'NONE', #14155, 11.68650000001168721 ) ;
#10246 = DIRECTION ( 'NONE',  ( 0.000000000000000000, 0.000000000000000000, -1.000000000000000000 ) ) ;
#10247 = VERTEX_POINT ( 'NONE', #2054 ) ;
#10248 = CIRCLE ( 'NONE', #19631, 8.999999999999994671 ) ;
#10249 = ADVANCED_FACE ( 'NONE', ( #123 ), #5373, .F. ) ;
#10250 = CIRCLE ( 'NONE', #16490, 5.000000000000007994 ) ;
#10251 = CARTESIAN_POINT ( 'NONE',  ( 64.69295543108962931, 5.000000000000007105, 6.123233995736765296E-16 ) ) ;
#10252 = AXIS2_PLACEMENT_3D ( 'NONE', #9588, #18523, #4122 ) ;
#10253 = ADVANCED_FACE ( 'NONE', ( #9479 ), #16937, .T. ) ;
#10254 = ORIENTED_EDGE ( 'NONE', *, *, #11767, .T. ) ;
#10255 = CARTESIAN_POINT ( 'NONE',  ( -9.500000000000000000, -6.482511860946779655E-13, -4.206742014460233214 ) ) ;
#10256 = VERTEX_POINT ( 'NONE', #14854 ) ;
#10257 = CARTESIAN_POINT ( 'NONE',  ( 77.48886275072855767, 7.562528597612068045E-15, 0.000000000000000000 ) ) ;
#10258 = CARTESIAN_POINT ( 'NONE',  ( -7.022953521754877748, -5.102474405760673015, 5.833165578109188232 ) ) ;
#10259 = VECTOR ( 'NONE', #9246, 1000.000000000000000 ) ;
#10260 = PLANE ( 'NONE',  #12732 ) ;
#10261 = LINE ( 'NONE', #428, #14988 ) ;
#10262 = CIRCLE ( 'NONE', #22748, 8.999999999999994671 ) ;
#10263 = ORIENTED_EDGE ( 'NONE', *, *, #21348, .F. ) ;
#10264 = CARTESIAN_POINT ( 'NONE',  ( 40.89823313241237912, 26.41789760203348081, 27.00000000000000000 ) ) ;
#10265 = EDGE_CURVE ( 'NONE', #581, #10236, #9253, .T. ) ;
#10266 = AXIS2_PLACEMENT_3D ( 'NONE', #11325, #13181, #16839 ) ;
#10267 = AXIS2_PLACEMENT_3D ( 'NONE', #8334, #6032, #4695 ) ;
#10268 = CARTESIAN_POINT ( 'NONE',  ( 2.935661446561383503, 9.035036904804158553, -5.606742014460233570 ) ) ;
#10269 = ORIENTED_EDGE ( 'NONE', *, *, #12549, .F. ) ;
#10270 = CIRCLE ( 'NONE', #23926, 49.99999999999999289 ) ;
#10271 = LINE ( 'NONE', #16005, #15350 ) ;
#10272 = EDGE_CURVE ( 'NONE', #10181, #18733, #881, .T. ) ;
#10273 = AXIS2_PLACEMENT_3D ( 'NONE', #16178, #1436, #14700 ) ;
#10274 = CARTESIAN_POINT ( 'NONE',  ( 0.000000000000000000, 0.000000000000000000, -3.000000000000000000 ) ) ;
#10275 = CIRCLE ( 'NONE', #11423, 5.000000000000007994 ) ;
#10276 = ORIENTED_EDGE ( 'NONE', *, *, #4485, .T. ) ;
#10277 = LINE ( 'NONE', #17860, #11205 ) ;
#10278 = ADVANCED_FACE ( 'NONE', ( #7657 ), #3890, .T. ) ;
#10279 = ORIENTED_EDGE ( 'NONE', *, *, #236, .T. ) ;
#10280 = CARTESIAN_POINT ( 'NONE',  ( 82.14750088563508257, 7.420530141404717394E-15, 0.000000000000000000 ) ) ;
#10281 = ADVANCED_FACE ( 'NONE', ( #24034 ), #7459, .F. ) ;
#10282 = CARTESIAN_POINT ( 'NONE',  ( -28.99999999999999645, 29.50000000000000000, 27.00000000000000000 ) ) ;
#10283 = CARTESIAN_POINT ( 'NONE',  ( -30.44534269664590553, 40.40463133211079594, 0.000000000000000000 ) ) ;
#10284 = DIRECTION ( 'NONE',  ( 0.000000000000000000, 0.000000000000000000, -1.000000000000000000 ) ) ;
#10285 = EDGE_LOOP ( 'NONE', ( #6974, #8102, #845, #9974, #12796, #8628 ) ) ;
#10286 = DIRECTION ( 'NONE',  ( 1.224646799147353207E-16, 1.000000000000000000, -0.000000000000000000 ) ) ;
#10287 = CARTESIAN_POINT ( 'NONE',  ( 81.27272727272728048, -4.172000000000000597, 5.616230220889771312E-16 ) ) ;
#10288 = DIRECTION ( 'NONE',  ( -1.000000000000000000, 0.000000000000000000, 0.000000000000000000 ) ) ;
#10289 = CARTESIAN_POINT ( 'NONE',  ( -5.871322893124554021, 8.081182679343978492, 4.759589141758144848 ) ) ;
#10290 = CIRCLE ( 'NONE', #16525, 9.000000000000000000 ) ;
#10291 = CIRCLE ( 'NONE', #8724, 9.999999999999998224 ) ;
#10292 = ORIENTED_EDGE ( 'NONE', *, *, #391, .T. ) ;
#10293 = EDGE_LOOP ( 'NONE', ( #7553, #3701, #1692, #4598, #21414, #974, #14164, #24068, #8941, #22564, #9560, #9508, #16708, #5047, #21109, #17646, #15032, #3356, #12633, #7344, #8755, #11145, #11146, #10901, #21758, #273, #1050, #4593, #23404, #9113, #12839, #10858, #20969 ) ) ;
#10294 = AXIS2_PLACEMENT_3D ( 'NONE', #12611, #20302, #16387 ) ;
#10295 = CIRCLE ( 'NONE', #16534, 2.024999999999999911 ) ;
#10296 = ORIENTED_EDGE ( 'NONE', *, *, #12992, .T. ) ;
#10297 = ORIENTED_EDGE ( 'NONE', *, *, #18584, .T. ) ;
#10298 = ORIENTED_EDGE ( 'NONE', *, *, #23354, .T. ) ;
#10299 = DIRECTION ( 'NONE',  ( 0.000000000000000000, -1.000000000000000000, 0.000000000000000000 ) ) ;
#10300 = CARTESIAN_POINT ( 'NONE',  ( -14.94708199919714176, -1.300481340138141872, -9.416259293296521449 ) ) ;
#10301 = DIRECTION ( 'NONE',  ( 1.000000000000000000, 2.600433232233976523E-16, -0.000000000000000000 ) ) ;
#10302 = ORIENTED_EDGE ( 'NONE', *, *, #16676, .T. ) ;
#10303 = LINE ( 'NONE', #8479, #9126 ) ;
#10304 = EDGE_CURVE ( 'NONE', #4131, #10954, #6318, .T. ) ;
#10305 = DIRECTION ( 'NONE',  ( 0.000000000000000000, -1.000000000000000000, 0.000000000000000000 ) ) ;
#10306 = EDGE_LOOP ( 'NONE', ( #18130, #7896, #231, #2860 ) ) ;
#10307 = CARTESIAN_POINT ( 'NONE',  ( 41.73082370883260239, 27.62204025492844650, -1.500000000000000000 ) ) ;
#10308 = LINE ( 'NONE', #15928, #12577 ) ;
#10309 = AXIS2_PLACEMENT_3D ( 'NONE', #12231, #2979, #16858 ) ;
#10310 = AXIS2_PLACEMENT_3D ( 'NONE', #7663, #20263, #3788 ) ;
#10311 = CARTESIAN_POINT ( 'NONE',  ( -10.83999999999999986, -14.99147757894464306, 0.000000000000000000 ) ) ;
#10312 = CARTESIAN_POINT ( 'NONE',  ( 3.890962118697714531E-15, 15.50000000000000000, 19.70000000000000284 ) ) ;
#10313 = CARTESIAN_POINT ( 'NONE',  ( 0.000000000000000000, 0.000000000000000000, -12.50000000000000000 ) ) ;
#10314 = VECTOR ( 'NONE', #10197, 1000.000000000000000 ) ;
#10315 = CARTESIAN_POINT ( 'NONE',  ( -31.74999999999995737, 0.000000000000000000, 5.000000000000000888 ) ) ;
#10316 = AXIS2_PLACEMENT_3D ( 'NONE', #21424, #6170, #19107 ) ;
#10317 = DIRECTION ( 'NONE',  ( 1.000000000000000000, 0.000000000000000000, 0.000000000000000000 ) ) ;
#10318 = CARTESIAN_POINT ( 'NONE',  ( 7.022953521755574080, -5.102474405759714671, -10.43316557810918788 ) ) ;
#10319 = AXIS2_PLACEMENT_3D ( 'NONE', #1902, #1449, #18501 ) ;
#10320 = DIRECTION ( 'NONE',  ( -0.5735764363510517105, -0.8191520442889879128, 0.000000000000000000 ) ) ;
#10321 = ORIENTED_EDGE ( 'NONE', *, *, #10039, .F. ) ;
#10322 = EDGE_LOOP ( 'NONE', ( #4499, #20435, #19554, #2830 ) ) ;
#10323 = CARTESIAN_POINT ( 'NONE',  ( 7.022953521755574080, -5.102474405759714671, 4.433165578109187877 ) ) ;
#10324 = B_SPLINE_CURVE_WITH_KNOTS ( 'NONE', 3,
 ( #19079, #8186, #13832, #4573, #534, #22873, #13327, #22741, #17108, #4078, #7952, #18834, #412, #16995, #15145, #6021, #9545, #22984, #15402, #6143, #4315, #11721 ),
 .UNSPECIFIED., .F., .F.,
 ( 4, 2, 2, 2, 2, 2, 2, 2, 2, 2, 4 ),
 ( 0.000000000000000000, 0.02930362155383451836, 0.05860724310766903672, 0.1172144862153381151, 0.1758217293230072142, 0.2344289724306762857, 0.2637325939845108769, 0.2930362155383454681, 0.3516434586460146505, 0.4102507017536837219, 0.4688579448613529044 ),
 .UNSPECIFIED. ) ;
#10325 = ORIENTED_EDGE ( 'NONE', *, *, #17, .T. ) ;
#10326 = DIRECTION ( 'NONE',  ( 0.9876466258105103257, 0.1566976149311594679, 0.000000000000000000 ) ) ;
#10327 =( BOUNDED_CURVE ( )  B_SPLINE_CURVE ( 2, ( #22157, #58, #7465, #5428, #16394, #23847, #14567, #22037, #13697, #3946, #20791 ),
 .UNSPECIFIED., .F., .T. ) 
 B_SPLINE_CURVE_WITH_KNOTS ( ( 3, 2, 2, 2, 2, 3 ),
 ( 0.2000000000000000111, 0.2200000000000000289, 0.2400000000000000466, 0.2600000000000000644, 0.2800000000000001377, 0.3000000000000000999 ),
 .UNSPECIFIED. ) 
 CURVE ( )  GEOMETRIC_REPRESENTATION_ITEM ( )  RATIONAL_B_SPLINE_CURVE ( ( 1.000000000000000000, 0.9510565162951535312, 1.000000000000000000, 0.9510565162951535312, 1.000000000000000000, 0.9510565162951535312, 1.000000000000000000, 0.9510565162951535312, 1.000000000000000000, 0.9510565162951533091, 1.000000000000000222 ) ) 
 REPRESENTATION_ITEM ( '' )  );
#10328 = DIRECTION ( 'NONE',  ( 0.7071067811865492381, 0.000000000000000000, 0.7071067811865457964 ) ) ;
#10329 = EDGE_LOOP ( 'NONE', ( #21490, #8923, #21731, #16842 ) ) ;
#10330 = CARTESIAN_POINT ( 'NONE',  ( -2.935661446561384391, -9.035036904804158553, -11.45958914175814414 ) ) ;
#10331 = AXIS2_PLACEMENT_3D ( 'NONE', #13578, #774, #11483 ) ;
#10332 = CARTESIAN_POINT ( 'NONE',  ( -1.000000000000000222, 0.000000000000000000, 3.699999999999998845 ) ) ;
#10333 = CARTESIAN_POINT ( 'NONE',  ( 3.890962118697714531E-15, 15.50000000000000000, 16.70000000000000284 ) ) ;
#10334 = CARTESIAN_POINT ( 'NONE',  ( 3.890962118697714531E-15, 15.50000000000000000, 19.70000000000000284 ) ) ;
#10335 = ADVANCED_FACE ( 'NONE', ( #22811 ), #20862, .T. ) ;
#10336 = ADVANCED_FACE ( 'NONE', ( #13532 ), #21345, .T. ) ;
#10337 = AXIS2_PLACEMENT_3D ( 'NONE', #6336, #15727, #12310 ) ;
#10338 = ORIENTED_EDGE ( 'NONE', *, *, #988, .T. ) ;
#10339 = AXIS2_PLACEMENT_3D ( 'NONE', #18909, #2190, #15210 ) ;
#10340 = DIRECTION ( 'NONE',  ( 1.000000000000000000, 0.000000000000000000, 0.000000000000000000 ) ) ;
#10341 = FACE_OUTER_BOUND ( 'NONE', #13248, .T. ) ;
#10342 = CARTESIAN_POINT ( 'NONE',  ( 41.73082370883257397, -29.49999999999999645, -1.500000000000000000 ) ) ;
#10343 = DIRECTION ( 'NONE',  ( -0.000000000000000000, -0.000000000000000000, -1.000000000000000000 ) ) ;
#10344 = CARTESIAN_POINT ( 'NONE',  ( -14.51962751333973856, 3.765689428759025681, 8.721787840009204373 ) ) ;
#10345 = CARTESIAN_POINT ( 'NONE',  ( 3.530011532367169913, 1.376079757590787351E-15, -11.23654394515110511 ) ) ;
#10346 = ORIENTED_EDGE ( 'NONE', *, *, #10714, .F. ) ;
#10347 = CARTESIAN_POINT ( 'NONE',  ( -2.682529543899159208, -8.255977015246598327, -4.033165578109189298 ) ) ;
#10348 = AXIS2_PLACEMENT_3D ( 'NONE', #14174, #1252, #1023 ) ;
#10349 = ORIENTED_EDGE ( 'NONE', *, *, #4163, .T. ) ;
#10350 = AXIS2_PLACEMENT_3D ( 'NONE', #3524, #12312, #18053 ) ;
#10351 = ORIENTED_EDGE ( 'NONE', *, *, #11463, .F. ) ;
#10352 = CARTESIAN_POINT ( 'NONE',  ( -7.685661446561619314, -5.583959896779019161, 5.259589141758143960 ) ) ;
#10353 = CARTESIAN_POINT ( 'NONE',  ( 2.935661446562616295, -9.035036904803758873, 10.80674201446023197 ) ) ;
#10354 = AXIS2_PLACEMENT_3D ( 'NONE', #15810, #21788, #21547 ) ;
#10355 = ORIENTED_EDGE ( 'NONE', *, *, #6733, .T. ) ;
#10356 =( NAMED_UNIT ( * ) SI_UNIT ( $, .STERADIAN. ) SOLID_ANGLE_UNIT ( ) );
#10357 = AXIS2_PLACEMENT_3D ( 'NONE', #15786, #10029, #14310 ) ;
#10358 = CARTESIAN_POINT ( 'NONE',  ( -2.024999999999999911, -45.00000000000000000, -3.000000000000000000 ) ) ;
#10359 = ADVANCED_FACE ( 'NONE', ( #11926 ), #15469, .F. ) ;
#10360 = CYLINDRICAL_SURFACE ( 'NONE', #2581, 4.499999999999997335 ) ;
#10361 = CARTESIAN_POINT ( 'NONE',  ( -40.23082370883257397, -29.50000000000000711, -3.000000000000000000 ) ) ;
#10362 = ADVANCED_FACE ( 'NONE', ( #19137 ), #5155, .T. ) ;
#10363 = CARTESIAN_POINT ( 'NONE',  ( 29.00000000000000000, 29.50000000000000000, -2.224999999999995204 ) ) ;
#10364 = LINE ( 'NONE', #12316, #491 ) ;
#10365 = EDGE_CURVE ( 'NONE', #1231, #16095, #13322, .T. ) ;
#10366 = EDGE_CURVE ( 'NONE', #3687, #5547, #18903, .T. ) ;
#10367 = AXIS2_PLACEMENT_3D ( 'NONE', #13607, #17503, #804 ) ;
#10368 = EDGE_CURVE ( 'NONE', #14422, #20068, #18786, .T. ) ;
#10369 = AXIS2_PLACEMENT_3D ( 'NONE', #584, #17525, #20961 ) ;
#10370 = DIRECTION ( 'NONE',  ( 1.000000000000000000, 0.000000000000000000, 0.000000000000000000 ) ) ;
#10371 = EDGE_LOOP ( 'NONE', ( #19765, #14195, #6294, #21117 ) ) ;
#10372 = AXIS2_PLACEMENT_3D ( 'NONE', #432, #18988, #22895 ) ;
#10373 = DIRECTION ( 'NONE',  ( -0.000000000000000000, -0.000000000000000000, 1.000000000000000000 ) ) ;
#10374 = DIRECTION ( 'NONE',  ( 0.000000000000000000, 1.000000000000000000, 0.000000000000000000 ) ) ;
#10375 = CARTESIAN_POINT ( 'NONE',  ( -40.29291594121673370, -26.62062637246459929, 11.00000000000000000 ) ) ;
#10376 = DIRECTION ( 'NONE',  ( -0.000000000000000000, -0.000000000000000000, -1.000000000000000000 ) ) ;
#10377 = DIRECTION ( 'NONE',  ( 0.000000000000000000, 0.000000000000000000, -1.000000000000000000 ) ) ;
#10378 = VECTOR ( 'NONE', #17346, 1000.000000000000000 ) ;
#10379 = DIRECTION ( 'NONE',  ( 0.5735764363510424957, 0.8191520442889943521, 0.000000000000000000 ) ) ;
#10380 = ORIENTED_EDGE ( 'NONE', *, *, #11286, .T. ) ;
#10381 = FACE_OUTER_BOUND ( 'NONE', #12460, .T. ) ;
#10382 = ORIENTED_EDGE ( 'NONE', *, *, #2629, .F. ) ;
#10383 = LINE ( 'NONE', #16346, #20451 ) ;
#10384 = ORIENTED_EDGE ( 'NONE', *, *, #4465, .T. ) ;
#10385 = CARTESIAN_POINT ( 'NONE',  ( 8.680847955710813579, 2.820578480814259326, 4.733165578109188587 ) ) ;
#10386 = CIRCLE ( 'NONE', #19763, 6.050000000006052758 ) ;
#10387 = DIRECTION ( 'NONE',  ( 0.000000000000000000, -1.000000000000000000, 0.000000000000000000 ) ) ;
#10388 = FACE_OUTER_BOUND ( 'NONE', #12330, .T. ) ;
#10389 = DIRECTION ( 'NONE',  ( 0.000000000000000000, 0.000000000000000000, 1.000000000000000000 ) ) ;
#10390 = ADVANCED_FACE ( 'NONE', ( #17428 ), #4147, .F. ) ;
#10391 = AXIS2_PLACEMENT_3D ( 'NONE', #21130, #4436, #11851 ) ;
#10392 = CARTESIAN_POINT ( 'NONE',  ( 0.000000000000000000, 0.000000000000000000, 11.22592346138681130 ) ) ;
#10393 = AXIS2_PLACEMENT_3D ( 'NONE', #9124, #20134, #18049 ) ;
#10394 = ORIENTED_EDGE ( 'NONE', *, *, #17130, .T. ) ;
#10395 = EDGE_CURVE ( 'NONE', #7322, #15518, #10590, .T. ) ;
#10396 = VERTEX_POINT ( 'NONE', #9969 ) ;
#10397 = EDGE_CURVE ( 'NONE', #14009, #23700, #837, .T. ) ;
#10398 = CARTESIAN_POINT ( 'NONE',  ( 0.000000000000000000, 0.000000000000000000, 0.000000000000000000 ) ) ;
#10399 = ADVANCED_FACE ( 'NONE', ( #356 ), #4400, .T. ) ;
#10400 = CARTESIAN_POINT ( 'NONE',  ( 6.809999908187194197E-13, -9.988891130263535700, -4.706742014460233214 ) ) ;
#10401 = ORIENTED_EDGE ( 'NONE', *, *, #18146, .T. ) ;
#10402 = ORIENTED_EDGE ( 'NONE', *, *, #12787, .F. ) ;
#10403 = CARTESIAN_POINT ( 'NONE',  ( -7.966265201740081459, -4.769768961436826160, -12.22297199169018711 ) ) ;
#10404 = CARTESIAN_POINT ( 'NONE',  ( -28.99999999999999645, -29.50000000000001066, 27.00000000000000000 ) ) ;
#10405 = ORIENTED_EDGE ( 'NONE', *, *, #14997, .F. ) ;
#10406 = DIRECTION ( 'NONE',  ( -1.000000000000000000, -0.000000000000000000, -0.000000000000000000 ) ) ;
#10407 = AXIS2_PLACEMENT_3D ( 'NONE', #12217, #15894, #8673 ) ;
#10408 = ORIENTED_EDGE ( 'NONE', *, *, #8031, .T. ) ;
#10409 = DIRECTION ( 'NONE',  ( 1.000000000000000000, 0.000000000000000000, 0.000000000000000000 ) ) ;
#10410 = PRODUCT ( 'socket head cap screw_iso_ISO 4762 M10 x 80 - 32S', 'socket head cap screw_iso_ISO 4762 M10 x 80 - 32S', '', ( #20678 ) ) ;
#10411 = CARTESIAN_POINT ( 'NONE',  ( 23.00000000000000000, 0.000000000000000000, 0.000000000000000000 ) ) ;
#10412 = CARTESIAN_POINT ( 'NONE',  ( 66.14750088563508257, 6.123233995736675563E-16, -5.000000000000007994 ) ) ;
#10413 = CARTESIAN_POINT ( 'NONE',  ( -20.85000000000000497, 15.03999999999999915, 0.000000000000000000 ) ) ;
#10414 = ORIENTED_EDGE ( 'NONE', *, *, #1728, .T. ) ;
#10415 = CARTESIAN_POINT ( 'NONE',  ( 61.78386452199871570, -4.999999999999999112, 0.000000000000000000 ) ) ;
#10416 = CARTESIAN_POINT ( 'NONE',  ( 23.90000000000000924, -29.50000000000000711, 27.00000000000000000 ) ) ;
#10417 = CARTESIAN_POINT ( 'NONE',  ( -6.822232771736903637E-13, 9.988891130263535700, 8.559589141758145558 ) ) ;
#10418 = ORIENTED_EDGE ( 'NONE', *, *, #7916, .F. ) ;
#10419 = EDGE_LOOP ( 'NONE', ( #8830, #14999, #15692, #17857 ) ) ;
#10420 = ORIENTED_EDGE ( 'NONE', *, *, #18530, .F. ) ;
#10421 = CARTESIAN_POINT ( 'NONE',  ( -1.999999999999994449, -45.00000000000000000, 27.00000000000000000 ) ) ;
#10422 = EDGE_CURVE ( 'NONE', #12203, #16008, #8257, .T. ) ;
#10423 = DIRECTION ( 'NONE',  ( -1.000000000000000000, 0.000000000000000000, 0.000000000000000000 ) ) ;
#10424 = DIRECTION ( 'NONE',  ( -1.000000000000000000, 0.000000000000000000, 0.000000000000000000 ) ) ;
#10425 = B_SPLINE_CURVE_WITH_KNOTS ( 'NONE', 3,
 ( #15934, #23281, #6556, #10436, #6434, #16044, #4725, #17634 ),
 .UNSPECIFIED., .F., .F.,
 ( 4, 2, 2, 4 ),
 ( 0.003892319173193294762, 0.004864202078960318081, 0.005836084984727341399, 0.007779850796261386300 ),
 .UNSPECIFIED. ) ;
#10426 = CARTESIAN_POINT ( 'NONE',  ( 0.2999999999999999889, 0.000000000000000000, 0.000000000000000000 ) ) ;
#10427 = ORIENTED_EDGE ( 'NONE', *, *, #9968, .F. ) ;
#10428 = FACE_OUTER_BOUND ( 'NONE', #15647, .T. ) ;
#10429 = CARTESIAN_POINT ( 'NONE',  ( -34.00000000000000000, -5.999999999999999112, 12.00000000000000000 ) ) ;
#10430 = CARTESIAN_POINT ( 'NONE',  ( 9.499999999999790390, 3.086737114213260025, 5.306742014460231971 ) ) ;
#10431 = DIRECTION ( 'NONE',  ( -1.000000000000000000, 0.000000000000000000, 0.000000000000000000 ) ) ;
#10432 = CARTESIAN_POINT ( 'NONE',  ( -9.500000000000202505, 3.086737114211975275, 4.959589141758144137 ) ) ;
#10433 = CARTESIAN_POINT ( 'NONE',  ( 89.12522638709219791, -1.078520768856852078E-29, 5.000000000000007994 ) ) ;
#10434 = LINE ( 'NONE', #21434, #8387 ) ;
#10435 = VECTOR ( 'NONE', #16645, 1000.000000000000000 ) ;
#10436 = CARTESIAN_POINT ( 'NONE',  ( 14.94777716362148645, 1.291632522116896054, 9.417361603030277806 ) ) ;
#10437 = CARTESIAN_POINT ( 'NONE',  ( 7.022953521755574080, -5.102474405759714671, -4.433165578109187877 ) ) ;
#10438 = EDGE_CURVE ( 'NONE', #5080, #498, #23176, .T. ) ;
#10439 = ORIENTED_EDGE ( 'NONE', *, *, #8555, .T. ) ;
#10440 = LINE ( 'NONE', #17901, #15999 ) ;
#10441 = ORIENTED_EDGE ( 'NONE', *, *, #21704, .T. ) ;
#10442 = EDGE_CURVE ( 'NONE', #9249, #13648, #472, .T. ) ;
#10443 = CARTESIAN_POINT ( 'NONE',  ( -7.022953521754877748, -5.102474405760673015, 5.833165578109188232 ) ) ;
#10444 = ORIENTED_EDGE ( 'NONE', *, *, #7347, .T. ) ;
#10445 = APPLICATION_PROTOCOL_DEFINITION ( 'draft international standard', 'automotive_design', 1998, #13193 ) ;
#10446 = ADVANCED_FACE ( 'NONE', ( #19270 ), #8134, .F. ) ;
#10447 = FACE_OUTER_BOUND ( 'NONE', #8054, .T. ) ;
#10448 = ORIENTED_EDGE ( 'NONE', *, *, #8969, .T. ) ;
#10449 = EDGE_CURVE ( 'NONE', #8760, #22901, #13768, .T. ) ;
#10450 = LINE ( 'NONE', #4986, #12652 ) ;
#10451 = CARTESIAN_POINT ( 'NONE',  ( -5.871322893123450015, -8.081182679344781405, -9.359589141758146269 ) ) ;
#10452 = AXIS2_PLACEMENT_3D ( 'NONE', #17026, #7849, #6172 ) ;
#10453 = AXIS2_PLACEMENT_3D ( 'NONE', #22236, #5506, #14882 ) ;
#10454 = CARTESIAN_POINT ( 'NONE',  ( 1.506443932848089640, 8.874555434635171380, 101.6016380241430568 ) ) ;
#10455 = FACE_OUTER_BOUND ( 'NONE', #12247, .T. ) ;
#10456 = DIRECTION ( 'NONE',  ( 0.000000000000000000, 1.000000000000000000, 0.000000000000000000 ) ) ;
#10457 = FACE_OUTER_BOUND ( 'NONE', #17381, .T. ) ;
#10458 = DIRECTION ( 'NONE',  ( -0.8247505806839237064, -0.5654966663575754504, 0.000000000000000000 ) ) ;
#10459 = CIRCLE ( 'NONE', #12837, 20.85000000000000142 ) ;
#10460 = DIRECTION ( 'NONE',  ( -1.000000000000000000, -1.224606353822377258E-16, -0.000000000000000000 ) ) ;
#10461 = ORIENTED_EDGE ( 'NONE', *, *, #11382, .F. ) ;
#10462 = LINE ( 'NONE', #23538, #15258 ) ;
#10463 = DIRECTION ( 'NONE',  ( -1.000000000000000000, -0.000000000000000000, -0.000000000000000000 ) ) ;
#10464 = CARTESIAN_POINT ( 'NONE',  ( -36.00000000000001421, 50.99999999999999289, 0.5000000000000000000 ) ) ;
#10465 = ORIENTED_EDGE ( 'NONE', *, *, #23260, .T. ) ;
#10466 = CARTESIAN_POINT ( 'NONE',  ( -8.680847955711200825, 2.820578480813073607, -5.533165578109187521 ) ) ;
#10467 =( BOUNDED_CURVE ( )  B_SPLINE_CURVE ( 2, ( #15930, #21550, #2387, #22904, #17510, #21316, #4353 ),
 .UNSPECIFIED., .F., .T. ) 
 B_SPLINE_CURVE_WITH_KNOTS ( ( 3, 2, 2, 3 ),
 ( 0.8000000000000000444, 0.8199999999999999512, 0.8399999999999999689, 0.8558632199373861216 ),
 .UNSPECIFIED. ) 
 CURVE ( )  GEOMETRIC_REPRESENTATION_ITEM ( )  RATIONAL_B_SPLINE_CURVE ( ( 1.000000000000000000, 0.9510565162951535312, 1.000000000000000000, 0.9510565162951535312, 1.000000000000000000, 0.9611799376744073475, 0.9839409940142059829 ) ) 
 REPRESENTATION_ITEM ( '' )  );
#10468 = ORIENTED_EDGE ( 'NONE', *, *, #10596, .T. ) ;
#10469 = ORIENTED_EDGE ( 'NONE', *, *, #7347, .F. ) ;
#10470 = CARTESIAN_POINT ( 'NONE',  ( -1.504652183083727168, 9.499999999999904077, 2.610843423304989308 ) ) ;
#10471 = ADVANCED_FACE ( 'NONE', ( #10085 ), #1333, .F. ) ;
#10472 = CARTESIAN_POINT ( 'NONE',  ( -2.935661446562617183, 9.035036904803758873, 9.806742014460233747 ) ) ;
#10473 = EDGE_CURVE ( 'NONE', #21725, #4506, #3204, .T. ) ;
#10474 = ORIENTED_EDGE ( 'NONE', *, *, #7829, .F. ) ;
#10475 = DIRECTION ( 'NONE',  ( -0.7052211081716895924, -0.7089874389501509278, 0.000000000000000000 ) ) ;
#10476 = DIRECTION ( 'NONE',  ( -1.000000000000000000, -0.000000000000000000, -0.000000000000000000 ) ) ;
#10477 = DIRECTION ( 'NONE',  ( -1.000000000000000000, 0.000000000000000000, 0.000000000000000000 ) ) ;
#10478 = DIRECTION ( 'NONE',  ( 1.000000000000000000, 0.000000000000000000, -0.000000000000000000 ) ) ;
#10479 = VECTOR ( 'NONE', #3919, 1000.000000000000000 ) ;
#10480 = ADVANCED_BREP_SHAPE_REPRESENTATION ( '', ( #18364, #8005 ), #15828 ) ;
#10481 = SURFACE_STYLE_FILL_AREA ( #5018 ) ;
#10482 = CARTESIAN_POINT ( 'NONE',  ( 60.90909090909091361, 7.491529369508391930E-15, 0.000000000000000000 ) ) ;
#10483 = ORIENTED_EDGE ( 'NONE', *, *, #6050, .T. ) ;
#10484 = CARTESIAN_POINT ( 'NONE',  ( 0.000000000000000000, 0.000000000000000000, 12.50000000000000000 ) ) ;
#10485 = DIRECTION ( 'NONE',  ( 1.000000000000000000, 0.000000000000000000, -0.000000000000000000 ) ) ;
#10486 = DIRECTION ( 'NONE',  ( -0.000000000000000000, 0.000000000000000000, 1.000000000000000000 ) ) ;
#10487 =( LENGTH_UNIT ( ) NAMED_UNIT ( * ) SI_UNIT ( .MILLI., .METRE. ) );
#10488 = EDGE_CURVE ( 'NONE', #23756, #6680, #23084, .T. ) ;
#10489 = CYLINDRICAL_SURFACE ( 'NONE', #19093, 4.999999999999997335 ) ;
#10490 = ORIENTED_EDGE ( 'NONE', *, *, #13807, .F. ) ;
#10491 = LINE ( 'NONE', #20261, #17751 ) ;
#10492 = EDGE_CURVE ( 'NONE', #17642, #14945, #10462, .T. ) ;
#10493 = ORIENTED_EDGE ( 'NONE', *, *, #16476, .T. ) ;
#10494 = DIRECTION ( 'NONE',  ( 0.000000000000000000, 0.000000000000000000, -1.000000000000000000 ) ) ;
#10495 = ORIENTED_EDGE ( 'NONE', *, *, #391, .F. ) ;
#10496 = CIRCLE ( 'NONE', #18688, 11.24716442891539714 ) ;
#10497 = DIRECTION ( 'NONE',  ( 0.000000000000000000, -1.000000000000000000, 0.000000000000000000 ) ) ;
#10498 = ADVANCED_FACE ( 'NONE', ( #10569 ), #18034, .F. ) ;
#10499 = EDGE_CURVE ( 'NONE', #19529, #10789, #6938, .T. ) ;
#10500 = ORIENTED_EDGE ( 'NONE', *, *, #5818, .T. ) ;
#10501 = DIRECTION ( 'NONE',  ( -0.000000000000000000, -0.000000000000000000, -1.000000000000000000 ) ) ;
#10502 = DIRECTION ( 'NONE',  ( 1.000000000000000000, 0.000000000000000000, 0.000000000000000000 ) ) ;
#10503 = CYLINDRICAL_SURFACE ( 'NONE', #7970, 4.999999999999997335 ) ;
#10504 = DIRECTION ( 'NONE',  ( 0.000000000000000000, -1.000000000000000000, 0.000000000000000000 ) ) ;
#10505 = VECTOR ( 'NONE', #3250, 1000.000000000000000 ) ;
#10506 = CARTESIAN_POINT ( 'NONE',  ( -9.500000000000000000, -6.482511860946779655E-13, -6.206742014460234103 ) ) ;
#10507 = ORIENTED_EDGE ( 'NONE', *, *, #8090, .F. ) ;
#10508 = ORIENTED_EDGE ( 'NONE', *, *, #10655, .T. ) ;
#10509 = CARTESIAN_POINT ( 'NONE',  ( 0.2211988718727270209, -9.109688270588595316, -12.42028818705274773 ) ) ;
#10510 = AXIS2_PLACEMENT_3D ( 'NONE', #639, #8048, #15492 ) ;
#10511 = CARTESIAN_POINT ( 'NONE',  ( 30.68762588338048403, 45.64284848299539732, -1.500000000000000000 ) ) ;
#10512 = CARTESIAN_POINT ( 'NONE',  ( -39.99999999999999289, -29.50000000000001066, 27.00000000000000000 ) ) ;
#10513 = EDGE_CURVE ( 'NONE', #2386, #2779, #12539, .T. ) ;
#10514 = EDGE_LOOP ( 'NONE', ( #1306, #8386, #13679, #15646 ) ) ;
#10515 = FACE_OUTER_BOUND ( 'NONE', #23293, .T. ) ;
#10516 = DIRECTION ( 'NONE',  ( -1.000000000000000000, -0.000000000000000000, -0.000000000000000000 ) ) ;
#10517 = CARTESIAN_POINT ( 'NONE',  ( 85.05659179472598908, 6.123233995736675563E-16, -5.000000000000007994 ) ) ;
#10518 = ORIENTED_EDGE ( 'NONE', *, *, #2996, .F. ) ;
#10519 = CARTESIAN_POINT ( 'NONE',  ( 5.871322893123448239, 8.081182679344781405, -9.506742014460231260 ) ) ;
#10520 = FACE_OUTER_BOUND ( 'NONE', #19633, .T. ) ;
#10521 = ADVANCED_FACE ( 'NONE', ( #21817 ), #16072, .T. ) ;
#10522 = CARTESIAN_POINT ( 'NONE',  ( -40.00000000000000000, 29.49999999999999645, 0.000000000000000000 ) ) ;
#10523 = ADVANCED_FACE ( 'NONE', ( #14359 ), #23769, .T. ) ;
#10524 = CARTESIAN_POINT ( 'NONE',  ( -6.153822176767817416E-13, 9.500000000000000000, 2.559589141758142450 ) ) ;
#10525 = AXIS2_PLACEMENT_3D ( 'NONE', #5514, #11222, #6004 ) ;
#10526 = EDGE_LOOP ( 'NONE', ( #7511, #20334, #1115, #14781, #8025, #802 ) ) ;
#10527 = ORIENTED_EDGE ( 'NONE', *, *, #6503, .T. ) ;
#10528 = EDGE_LOOP ( 'NONE', ( #9977, #7473, #7259, #14539 ) ) ;
#10529 = DIRECTION ( 'NONE',  ( -0.000000000000000000, -0.000000000000000000, -1.000000000000000000 ) ) ;
#10530 = DIRECTION ( 'NONE',  ( -1.000000000000000000, 0.000000000000000000, 0.000000000000000000 ) ) ;
#10531 = DIRECTION ( 'NONE',  ( -0.000000000000000000, -0.000000000000000000, 1.000000000000000000 ) ) ;
#10532 = ORIENTED_EDGE ( 'NONE', *, *, #15252, .T. ) ;
#10533 = DIRECTION ( 'NONE',  ( -0.000000000000000000, -0.000000000000000000, -1.000000000000000000 ) ) ;
#10534 = CARTESIAN_POINT ( 'NONE',  ( 0.000000000000000000, -13.66196005206966468, 3.918670437617043145 ) ) ;
#10535 = EDGE_LOOP ( 'NONE', ( #2496, #3730, #11489, #806 ) ) ;
#10536 = DIRECTION ( 'NONE',  ( 1.000000000000000000, 1.224606353822377258E-16, 0.000000000000000000 ) ) ;
#10537 = DIRECTION ( 'NONE',  ( 0.9160001545545232160, 0.4011779117250717785, 0.000000000000000000 ) ) ;
#10538 = CARTESIAN_POINT ( 'NONE',  ( -9.500000000000211386, 3.086737114211961064, 4.106742014460232681 ) ) ;
#10539 = VECTOR ( 'NONE', #4859, 1000.000000000000000 ) ;
#10540 = FACE_OUTER_BOUND ( 'NONE', #5382, .T. ) ;
#10541 = CARTESIAN_POINT ( 'NONE',  ( -6.822232771736904647E-13, 9.988891130263535700, 4.559589141758142894 ) ) ;
#10542 = CARTESIAN_POINT ( 'NONE',  ( 17.49066032632880408, -9.200828712690857003, -2.414248458042545842 ) ) ;
#10543 = CARTESIAN_POINT ( 'NONE',  ( 84.76159002345582394, -5.000000000000000888, 6.123233995736776143E-16 ) ) ;
#10544 = FACE_OUTER_BOUND ( 'NONE', #11079, .T. ) ;
#10545 = EDGE_CURVE ( 'NONE', #5796, #17727, #4754, .T. ) ;
#10546 = EDGE_CURVE ( 'NONE', #5547, #8536, #21539, .T. ) ;
#10547 = ORIENTED_EDGE ( 'NONE', *, *, #15266, .T. ) ;
#10548 = CARTESIAN_POINT ( 'NONE',  ( -8.680847955711200825, 2.820578480813073607, 9.533165578109187521 ) ) ;
#10549 = ORIENTED_EDGE ( 'NONE', *, *, #3584, .T. ) ;
#10550 = CARTESIAN_POINT ( 'NONE',  ( 8.680847955711007202, 5.912916378492122225E-13, 6.633165578109188942 ) ) ;
#10551 = DIRECTION ( 'NONE',  ( 0.000000000000000000, 0.000000000000000000, 1.000000000000000000 ) ) ;
#10552 = CARTESIAN_POINT ( 'NONE',  ( 40.00000000000000000, -29.49999999999999645, 11.00000000000000000 ) ) ;
#10553 = CIRCLE ( 'NONE', #23823, 8.000000000000007105 ) ;
#10554 = VERTEX_POINT ( 'NONE', #19641 ) ;
#10555 = CARTESIAN_POINT ( 'NONE',  ( 5.000000000000000000, 4.685197434473818312, -1.301042606982605321E-15 ) ) ;
#10556 = CARTESIAN_POINT ( 'NONE',  ( 5.871322893124553133, -8.081182679343980269, -9.759589141758143072 ) ) ;
#10557 = CIRCLE ( 'NONE', #16021, 5.000000000000007994 ) ;
#10558 = CARTESIAN_POINT ( 'NONE',  ( -6.153822176767817416E-13, 9.500000000000000000, 2.559589141758142894 ) ) ;
#10559 = DIRECTION ( 'NONE',  ( -0.1313947906041722513, -0.9913301211009810654, 0.000000000000000000 ) ) ;
#10560 = CARTESIAN_POINT ( 'NONE',  ( -34.10000000000000142, -29.49999999999999645, 0.000000000000000000 ) ) ;
#10561 = EDGE_CURVE ( 'NONE', #6803, #15584, #10973, .T. ) ;
#10562 = FACE_OUTER_BOUND ( 'NONE', #8587, .T. ) ;
#10563 = ORIENTED_EDGE ( 'NONE', *, *, #12129, .T. ) ;
#10564 = DIRECTION ( 'NONE',  ( -2.600433232233976523E-16, 1.000000000000000000, 0.000000000000000000 ) ) ;
#10565 = ADVANCED_FACE ( 'NONE', ( #3269 ), #21709, .F. ) ;
#10566 = CARTESIAN_POINT ( 'NONE',  ( 9.324366623732823450E-16, 111.0000000000000000, 77.99999999999998579 ) ) ;
#10567 = VERTEX_POINT ( 'NONE', #3145 ) ;
#10568 = DIRECTION ( 'NONE',  ( 1.000000000000000000, 0.000000000000000000, 0.000000000000000000 ) ) ;
#10569 = FACE_OUTER_BOUND ( 'NONE', #20124, .T. ) ;
#10570 = FACE_OUTER_BOUND ( 'NONE', #13114, .T. ) ;
#10571 = CARTESIAN_POINT ( 'NONE',  ( 17.19784311473120653, 8.411123426659424140, 4.422670359120418837 ) ) ;
#10572 = EDGE_CURVE ( 'NONE', #6675, #23304, #8757, .T. ) ;
#10573 = LINE ( 'NONE', #16423, #8345 ) ;
#10574 = VERTEX_POINT ( 'NONE', #18164 ) ;
#10575 = FACE_OUTER_BOUND ( 'NONE', #7091, .T. ) ;
#10576 = AXIS2_PLACEMENT_3D ( 'NONE', #5112, #20003, #9123 ) ;
#10577 = CARTESIAN_POINT ( 'NONE',  ( -2.935661446562617183, 9.035036904803758873, -9.806742014460233747 ) ) ;
#10578 = AXIS2_PLACEMENT_3D ( 'NONE', #13096, #3475, #14916 ) ;
#10579 = VERTEX_POINT ( 'NONE', #23664 ) ;
#10580 = ORIENTED_EDGE ( 'NONE', *, *, #21444, .T. ) ;
#10581 = CARTESIAN_POINT ( 'NONE',  ( -5.871322893124554021, 8.081182679343978492, 2.759589141758142627 ) ) ;
#10582 = CARTESIAN_POINT ( 'NONE',  ( -9.499999999999790390, -3.086737114213257804, 4.306742014460233747 ) ) ;
#10583 = ORIENTED_EDGE ( 'NONE', *, *, #20212, .T. ) ;
#10584 = FACE_OUTER_BOUND ( 'NONE', #20801, .T. ) ;
#10585 = CARTESIAN_POINT ( 'NONE',  ( 87.67068093254673045, 7.562528597612068045E-15, 0.000000000000000000 ) ) ;
#10586 = AXIS2_PLACEMENT_3D ( 'NONE', #13528, #22928, #17425 ) ;
#10587 = DIRECTION ( 'NONE',  ( 0.000000000000000000, -1.000000000000000000, 0.000000000000000000 ) ) ;
#10588 = DIRECTION ( 'NONE',  ( -0.000000000000000000, -0.000000000000000000, -1.000000000000000000 ) ) ;
#10589 = AXIS2_PLACEMENT_3D ( 'NONE', #22482, #22697, #9506 ) ;
#10590 = CIRCLE ( 'NONE', #8254, 5.025000000000002132 ) ;
#10591 = PRODUCT ( 'Assembly Lag Sleeve', 'Assembly Lag Sleeve', '', ( #2135 ) ) ;
#10592 = AXIS2_PLACEMENT_3D ( 'NONE', #8459, #6752, #6521 ) ;
#10593 = AXIS2_PLACEMENT_3D ( 'NONE', #8570, #23821, #10755 ) ;
#10594 = ORIENTED_EDGE ( 'NONE', *, *, #12940, .T. ) ;
#10595 = AXIS2_PLACEMENT_3D ( 'NONE', #1517, #12470, #19710 ) ;
#10596 = EDGE_CURVE ( 'NONE', #6874, #5306, #17226, .T. ) ;
#10597 = ORIENTED_EDGE ( 'NONE', *, *, #20818, .F. ) ;
#10598 =( LENGTH_UNIT ( ) NAMED_UNIT ( * ) SI_UNIT ( .MILLI., .METRE. ) );
#10599 = DIRECTION ( 'NONE',  ( -1.000000000000000000, 0.000000000000000000, 0.000000000000000000 ) ) ;
#10600 =( NAMED_UNIT ( * ) PLANE_ANGLE_UNIT ( ) SI_UNIT ( $, .RADIAN. ) );
#10601 = LINE ( 'NONE', #19423, #4294 ) ;
#10602 = LINE ( 'NONE', #21973, #13454 ) ;
#10603 = ORIENTED_EDGE ( 'NONE', *, *, #18122, .F. ) ;
#10604 = LINE ( 'NONE', #19905, #586 ) ;
#10605 = ORIENTED_EDGE ( 'NONE', *, *, #12454, .T. ) ;
#10606 = AXIS2_PLACEMENT_3D ( 'NONE', #12875, #20333, #20459 ) ;
#10607 = CARTESIAN_POINT ( 'NONE',  ( 20.85000000000000853, 15.03999999999999915, 25.00000000000000000 ) ) ;
#10608 = AXIS2_PLACEMENT_3D ( 'NONE', #636, #9872, #6607 ) ;
#10609 = CARTESIAN_POINT ( 'NONE',  ( 68.18181818181818699, 7.491529369508391930E-15, 0.000000000000000000 ) ) ;
#10610 = CIRCLE ( 'NONE', #12942, 4.249999999999996447 ) ;
#10611 = ORIENTED_EDGE ( 'NONE', *, *, #13314, .F. ) ;
#10612 = DIRECTION ( 'NONE',  ( -1.000000000000000000, 0.000000000000000000, 0.000000000000000000 ) ) ;
#10613 = VECTOR ( 'NONE', #159, 1000.000000000000000 ) ;
#10614 = DIRECTION ( 'NONE',  ( 0.000000000000000000, 0.000000000000000000, 1.000000000000000000 ) ) ;
#10615 = DIRECTION ( 'NONE',  ( 1.000000000000000000, 8.320016671351592327E-16, 0.000000000000000000 ) ) ;
#10616 = VECTOR ( 'NONE', #19732, 1000.000000000000000 ) ;
#10617 = DIRECTION ( 'NONE',  ( 0.000000000000000000, -1.000000000000000000, 0.000000000000000000 ) ) ;
#10618 = ORIENTED_EDGE ( 'NONE', *, *, #9003, .T. ) ;
#10619 = CARTESIAN_POINT ( 'NONE',  ( 0.000000000000000000, -45.00000000000000000, 3.000000000000002665 ) ) ;
#10620 = CARTESIAN_POINT ( 'NONE',  ( 59.45454545454545325, 7.491529369508391930E-15, 0.000000000000000000 ) ) ;
#10621 = EDGE_CURVE ( 'NONE', #20393, #18883, #9811, .T. ) ;
#10622 = ORIENTED_EDGE ( 'NONE', *, *, #12429, .T. ) ;
#10623 = EDGE_LOOP ( 'NONE', ( #8565, #15249, #4392, #20820 ) ) ;
#10624 = DIRECTION ( 'NONE',  ( -1.000000000000000000, 0.000000000000000000, 0.000000000000000000 ) ) ;
#10625 = VECTOR ( 'NONE', #16279, 1000.000000000000227 ) ;
#10626 = ADVANCED_FACE ( 'NONE', ( #2785 ), #2776, .F. ) ;
#10627 = CIRCLE ( 'NONE', #134, 17.87500000001787726 ) ;
#10628 = EDGE_CURVE ( 'NONE', #7385, #5720, #21087, .T. ) ;
#10629 = CARTESIAN_POINT ( 'NONE',  ( 28.27483331787888332, -41.23752903419610050, 27.00000000000000000 ) ) ;
#10630 = AXIS2_PLACEMENT_3D ( 'NONE', #8077, #4692, #10143 ) ;
#10631 = VERTEX_POINT ( 'NONE', #7162 ) ;
#10632 = VECTOR ( 'NONE', #22949, 1000.000000000000000 ) ;
#10633 = FACE_OUTER_BOUND ( 'NONE', #3574, .T. ) ;
#10634 = CARTESIAN_POINT ( 'NONE',  ( 88.54545454545454675, -4.172000000000000597, 5.616230220889771312E-16 ) ) ;
#10635 = ORIENTED_EDGE ( 'NONE', *, *, #2297, .F. ) ;
#10636 = CARTESIAN_POINT ( 'NONE',  ( 10.49999999999999822, 0.000000000000000000, 3.499999999999999556 ) ) ;
#10637 = FACE_OUTER_BOUND ( 'NONE', #10062, .T. ) ;
#10638 = CARTESIAN_POINT ( 'NONE',  ( 23.00000000000000000, 14.21257171757157955, -0.08908218613038007549 ) ) ;
#10639 = ORIENTED_EDGE ( 'NONE', *, *, #21834, .F. ) ;
#10640 = DIRECTION ( 'NONE',  ( 0.000000000000000000, -1.000000000000000000, 0.000000000000000000 ) ) ;
#10641 = VECTOR ( 'NONE', #13587, 1000.000000000000000 ) ;
#10642 = ORIENTED_EDGE ( 'NONE', *, *, #20717, .T. ) ;
#10643 = AXIS2_PLACEMENT_3D ( 'NONE', #3591, #20314, #194 ) ;
#10644 = ADVANCED_FACE ( 'NONE', ( #14600 ), #11270, .T. ) ;
#10645 = CIRCLE ( 'NONE', #153, 8.000000000000000000 ) ;
#10646 = AXIS2_PLACEMENT_3D ( 'NONE', #7339, #22240, #5406 ) ;
#10647 = ORIENTED_EDGE ( 'NONE', *, *, #9624, .T. ) ;
#10649 = VERTEX_POINT ( 'NONE', #5219 ) ;
#10648 = AXIS2_PLACEMENT_3D ( 'NONE', #7468, #22398, #5679 ) ;
#10650 = DIRECTION ( 'NONE',  ( -1.000000000000000000, -0.000000000000000000, -0.000000000000000000 ) ) ;
#10651 = EDGE_CURVE ( 'NONE', #15821, #6200, #23050, .T. ) ;
#10652 = CARTESIAN_POINT ( 'NONE',  ( 0.000000000000000000, -45.00000000000000000, -23.99999999999999645 ) ) ;
#10653 = ORIENTED_EDGE ( 'NONE', *, *, #1882, .T. ) ;
#10654 = ORIENTED_EDGE ( 'NONE', *, *, #6630, .F. ) ;
#10655 = EDGE_CURVE ( 'NONE', #17886, #22869, #5882, .T. ) ;
#10656 = EDGE_CURVE ( 'NONE', #3076, #1666, #19535, .T. ) ;
#10657 = EDGE_CURVE ( 'NONE', #12954, #22930, #2382, .T. ) ;
#10658 = DIRECTION ( 'NONE',  ( 0.8571673007021118895, 1.049727191138618079E-16, -0.5150380749100549327 ) ) ;
#10659 = ORIENTED_EDGE ( 'NONE', *, *, #24077, .T. ) ;
#10660 = FACE_OUTER_BOUND ( 'NONE', #10902, .T. ) ;
#10661 = CARTESIAN_POINT ( 'NONE',  ( 9.090423977855502713, 6.191897047423500831E-13, 12.34637735993366725 ) ) ;
#10662 = CARTESIAN_POINT ( 'NONE',  ( -5.871322893123450015, -8.081182679344781405, 4.506742014460231260 ) ) ;
#10663 = DIRECTION ( 'NONE',  ( -0.000000000000000000, -1.000000000000000000, -0.000000000000000000 ) ) ;
#10664 = DIRECTION ( 'NONE',  ( 1.000000000000000000, 0.000000000000000000, 0.000000000000000000 ) ) ;
#10665 = DIRECTION ( 'NONE',  ( -0.000000000000000000, -0.000000000000000000, -1.000000000000000000 ) ) ;
#10666 = CARTESIAN_POINT ( 'NONE',  ( -41.00000000000000000, -26.82133436441678853, 12.00000000000000000 ) ) ;
#10667 = VECTOR ( 'NONE', #18674, 1000.000000000000000 ) ;
#10668 = DIRECTION ( 'NONE',  ( 0.9945797436152715720, 0.1039766011667100365, -0.000000000000000000 ) ) ;
#10669 = AXIS2_PLACEMENT_3D ( 'NONE', #17486, #6642, #22992 ) ;
#10670 = DIRECTION ( 'NONE',  ( 0.000000000000000000, 1.000000000000000000, 0.000000000000000000 ) ) ;
#10671 = CONICAL_SURFACE ( 'NONE', #177, 4.172000000000008590, 0.9599310885968742602 ) ;
#10672 = AXIS2_PLACEMENT_3D ( 'NONE', #3682, #3329, #11094 ) ;
#10673 = CARTESIAN_POINT ( 'NONE',  ( -5.365059087799947335, 7.384370330706355290, 9.333165578109190008 ) ) ;
#10674 = ORIENTED_EDGE ( 'NONE', *, *, #11367, .F. ) ;
#10675 = PRODUCT_CONTEXT ( 'NONE', #10238, 'mechanical' ) ;
#10676 = EDGE_CURVE ( 'NONE', #8169, #7597, #10168, .T. ) ;
#10677 = PLANE ( 'NONE',  #17072 ) ;
#10678 = ORIENTED_EDGE ( 'NONE', *, *, #11142, .T. ) ;
#10679 = ORIENTED_EDGE ( 'NONE', *, *, #4394, .F. ) ;
#10680 = CARTESIAN_POINT ( 'NONE',  ( 42.00000000000000000, 3.999999999999987121, 8.500000000000000000 ) ) ;
#10681 = CARTESIAN_POINT ( 'NONE',  ( 9.499999999999790390, 3.086737114213260025, -8.159589141758143427 ) ) ;
#10682 = EDGE_CURVE ( 'NONE', #10927, #3165, #18358, .T. ) ;
#10683 = AXIS2_PLACEMENT_3D ( 'NONE', #5850, #1840, #10844 ) ;
#10684 = CARTESIAN_POINT ( 'NONE',  ( 2.382124412452373274, 8.679761848089601273, 100.8339782245926699 ) ) ;
#10685 = CARTESIAN_POINT ( 'NONE',  ( 28.73477696352899358, -42.73830357953205095, -1.500000000000000000 ) ) ;
#10686 = EDGE_CURVE ( 'NONE', #1010, #17386, #10557, .T. ) ;
#10687 = CIRCLE ( 'NONE', #5258, 5.100000000000000533 ) ;
#10688 = CARTESIAN_POINT ( 'NONE',  ( 90.00000000000000000, 0.000000000000000000, 0.000000000000000000 ) ) ;
#10689 = ORIENTED_EDGE ( 'NONE', *, *, #8778, .F. ) ;
#10690 = DIRECTION ( 'NONE',  ( -1.000000000000000000, -0.000000000000000000, -0.000000000000000000 ) ) ;
#10691 = VECTOR ( 'NONE', #18040, 1000.000000000000000 ) ;
#10692 = ORIENTED_EDGE ( 'NONE', *, *, #8901, .F. ) ;
#10693 = DIRECTION ( 'NONE',  ( -1.000000000000000000, 0.000000000000000000, 0.000000000000000000 ) ) ;
#10694 = DIRECTION ( 'NONE',  ( 0.000000000000000000, 0.000000000000000000, 1.000000000000000000 ) ) ;
#10695 = FACE_OUTER_BOUND ( 'NONE', #7869, .T. ) ;
#10696 = CARTESIAN_POINT ( 'NONE',  ( 16.18147534945000032, 6.260849737139247750, 7.148624562014526340 ) ) ;
#10697 = CONICAL_SURFACE ( 'NONE', #13438, 4.172000000000008590, 0.9599310885968742602 ) ;
#10698 = DIRECTION ( 'NONE',  ( -0.000000000000000000, -0.000000000000000000, -1.000000000000000000 ) ) ;
#10699 = EDGE_LOOP ( 'NONE', ( #21377, #13574, #16345, #22182 ) ) ;
#10700 = CARTESIAN_POINT ( 'NONE',  ( 37.00000000000000711, -29.50000000000000355, 11.50000000000000000 ) ) ;
#10701 = CARTESIAN_POINT ( 'NONE',  ( 31.49999999999999289, -51.00000000000000711, 0.5000000000000004441 ) ) ;
#10702 = EDGE_LOOP ( 'NONE', ( #17519, #7387, #16531, #13271 ) ) ;
#10703 = ORIENTED_EDGE ( 'NONE', *, *, #6763, .T. ) ;
#10704 = APPLICATION_CONTEXT ( 'automotive_design' ) ;
#10705 = CARTESIAN_POINT ( 'NONE',  ( 2.935661446562616295, -9.035036904803758873, 5.659589141758144315 ) ) ;
#10706 = CARTESIAN_POINT ( 'NONE',  ( 6.809999908187194197E-13, -9.988891130263535700, 8.706742014460230550 ) ) ;
#10707 = LINE ( 'NONE', #12661, #1432 ) ;
#10708 = ORIENTED_EDGE ( 'NONE', *, *, #18349, .F. ) ;
#10709 = CIRCLE ( 'NONE', #8770, 11.22592346138681130 ) ;
#10710 = EDGE_LOOP ( 'NONE', ( #20092, #2846, #11986, #18045, #22176 ) ) ;
#10711 = CARTESIAN_POINT ( 'NONE',  ( -9.500000000000000000, -6.482511860946779655E-13, -4.206742014460233214 ) ) ;
#10712 = CIRCLE ( 'NONE', #19693, 14.99999999999999822 ) ;
#10713 = FACE_OUTER_BOUND ( 'NONE', #11618, .T. ) ;
#10714 = EDGE_CURVE ( 'NONE', #1952, #1785, #1294, .T. ) ;
#10715 = CARTESIAN_POINT ( 'NONE',  ( 83.60204634018053582, 5.000000000000025757, 6.123233995736788962E-16 ) ) ;
#10716 = CARTESIAN_POINT ( 'NONE',  ( 11.50000000000000000, -7.033831428820292331, 16.43291941292170577 ) ) ;
#10717 = CIRCLE ( 'NONE', #9537, 8.000000000000003553 ) ;
#10718 = DIRECTION ( 'NONE',  ( -0.000000000000000000, -0.000000000000000000, -1.000000000000000000 ) ) ;
#10719 = CARTESIAN_POINT ( 'NONE',  ( 6.250000000000000000, 10.82531754730548279, -2.500000000000000000 ) ) ;
#10720 = EDGE_CURVE ( 'NONE', #10236, #780, #16789, .T. ) ;
#10721 = DIRECTION ( 'NONE',  ( 0.000000000000000000, 0.000000000000000000, 1.000000000000000000 ) ) ;
#10722 = DIRECTION ( 'NONE',  ( 0.5735764363510427177, -0.8191520442889941300, 1.003171929053527705E-16 ) ) ;
#10723 = DIRECTION ( 'NONE',  ( 1.000000000000000000, 0.000000000000000000, 0.000000000000000000 ) ) ;
#10724 = PRESENTATION_STYLE_ASSIGNMENT (( #15984 ) ) ;
#10725 = CARTESIAN_POINT ( 'NONE',  ( -5.796569164227505233, 7.552650514639522861, -3.500400752039017238 ) ) ;
#10726 = LINE ( 'NONE', #6965, #2517 ) ;
#10727 = VECTOR ( 'NONE', #10100, 1000.000000000000000 ) ;
#10728 = CARTESIAN_POINT ( 'NONE',  ( 64.39795365981944997, 7.562528597612068045E-15, 0.000000000000000000 ) ) ;
#10729 = CIRCLE ( 'NONE', #12684, 5.000000000000007994 ) ;
#10730 = LINE ( 'NONE', #5259, #15395 ) ;
#10731 = VERTEX_POINT ( 'NONE', #9105 ) ;
#10732 = DIRECTION ( 'NONE',  ( -0.000000000000000000, -0.000000000000000000, 1.000000000000000000 ) ) ;
#10733 = VERTEX_POINT ( 'NONE', #16677 ) ;
#10734 = CARTESIAN_POINT ( 'NONE',  ( 70.51113724927145654, 5.000000000000007105, 6.123233995736765296E-16 ) ) ;
#10735 = EDGE_CURVE ( 'NONE', #14009, #4656, #6685, .T. ) ;
#10736 = ORIENTED_EDGE ( 'NONE', *, *, #6468, .T. ) ;
#10737 = CARTESIAN_POINT ( 'NONE',  ( -1.999999999999994449, 45.00000000000000000, 26.97499999999999432 ) ) ;
#10738 = EDGE_CURVE ( 'NONE', #7598, #20616, #8975, .T. ) ;
#10739 = DIRECTION ( 'NONE',  ( 0.000000000000000000, 1.000000000000000000, 0.000000000000000000 ) ) ;
#10740 = VECTOR ( 'NONE', #3856, 1000.000000000000000 ) ;
#10741 = EDGE_CURVE ( 'NONE', #12778, #9530, #9759, .T. ) ;
#10742 = AXIS2_PLACEMENT_3D ( 'NONE', #19523, #2803, #6339 ) ;
#10743 = CARTESIAN_POINT ( 'NONE',  ( -41.00000000000000000, 5.000000000000000888, 11.00000000000000000 ) ) ;
#10744 = EDGE_CURVE ( 'NONE', #13405, #17352, #5459, .T. ) ;
#10745 = FACE_OUTER_BOUND ( 'NONE', #6296, .T. ) ;
#10746 = CIRCLE ( 'NONE', #14656, 1.999999999999997113 ) ;
#10747 = CARTESIAN_POINT ( 'NONE',  ( 7.685661446562381371, -5.583959896777971110, -11.85958914175814449 ) ) ;
#10748 = EDGE_LOOP ( 'NONE', ( #19567, #8858, #1217, #9652 ) ) ;
#10749 = ORIENTED_EDGE ( 'NONE', *, *, #15628, .T. ) ;
#10750 = CARTESIAN_POINT ( 'NONE',  ( -31.10231664966676135, -45.36128193761570770, 27.00000000000000000 ) ) ;
#10751 = FACE_OUTER_BOUND ( 'NONE', #9794, .T. ) ;
#10752 = DIRECTION ( 'NONE',  ( -1.000000000000000000, -1.224606353822377258E-16, -0.000000000000000000 ) ) ;
#10753 = ORIENTED_EDGE ( 'NONE', *, *, #7942, .F. ) ;
#10754 = CIRCLE ( 'NONE', #9589, 5.000000000000007994 ) ;
#10755 = DIRECTION ( 'NONE',  ( 1.000000000000000000, 0.000000000000000000, 0.000000000000000000 ) ) ;
#10756 =( GEOMETRIC_REPRESENTATION_CONTEXT ( 3 ) GLOBAL_UNCERTAINTY_ASSIGNED_CONTEXT ( ( #345 ) ) GLOBAL_UNIT_ASSIGNED_CONTEXT ( ( #9120, #20844, #7296 ) ) REPRESENTATION_CONTEXT ( 'NONE', 'WORKASPACE' ) );
#10757 = AXIS2_PLACEMENT_3D ( 'NONE', #2867, #5173, #15919 ) ;
#10758 = CARTESIAN_POINT ( 'NONE',  ( 80.39795365981946418, 6.123233995736675563E-16, -5.000000000000007994 ) ) ;
#10759 = ORIENTED_EDGE ( 'NONE', *, *, #23736, .F. ) ;
#10760 = CARTESIAN_POINT ( 'NONE',  ( 9.500000000000000000, 6.470877716354879437E-13, -9.206742014460234103 ) ) ;
#10761 = CARTESIAN_POINT ( 'NONE',  ( 0.000000000000000000, -15.23000000000000220, 27.00000000000000000 ) ) ;
#10762 = CARTESIAN_POINT ( 'NONE',  ( -40.66734255040739043, 26.56420859267092283, -3.000000000000000000 ) ) ;
#10763 = AXIS2_PLACEMENT_3D ( 'NONE', #2433, #22828, #6103 ) ;
#10764 = CYLINDRICAL_SURFACE ( 'NONE', #5118, 1.000000000000000000 ) ;
#10765 = EDGE_CURVE ( 'NONE', #8837, #1531, #20339, .T. ) ;
#10766 = EDGE_CURVE ( 'NONE', #3802, #11621, #19528, .T. ) ;
#10767 = VERTEX_POINT ( 'NONE', #10057 ) ;
#10768 = EDGE_LOOP ( 'NONE', ( #17638, #22084, #150 ) ) ;
#10769 = DIRECTION ( 'NONE',  ( 0.000000000000000000, -1.000000000000000000, 0.000000000000000000 ) ) ;
#10770 = AXIS2_PLACEMENT_3D ( 'NONE', #14649, #16124, #14399 ) ;
#10771 = LINE ( 'NONE', #9501, #19655 ) ;
#10772 = DIRECTION ( 'NONE',  ( -1.000000000000000000, 0.000000000000000000, 0.000000000000000000 ) ) ;
#10773 = EDGE_LOOP ( 'NONE', ( #22967, #4063, #22385, #6673 ) ) ;
#10774 = ORIENTED_EDGE ( 'NONE', *, *, #15125, .T. ) ;
#10775 = DIRECTION ( 'NONE',  ( -0.000000000000000000, -0.000000000000000000, -1.000000000000000000 ) ) ;
#10776 = VERTEX_POINT ( 'NONE', #9943 ) ;
#10777 = CARTESIAN_POINT ( 'NONE',  ( 35.99999999999992184, -60.00000000000000000, 12.50000000000000000 ) ) ;
#10778 = CARTESIAN_POINT ( 'NONE',  ( 9.500000000000000000, 6.470877716354879437E-13, 5.206742014460234103 ) ) ;
#10779 = CYLINDRICAL_SURFACE ( 'NONE', #23378, 8.000000000000000000 ) ;
#10780 = DIRECTION ( 'NONE',  ( -0.000000000000000000, 1.000000000000000000, -0.000000000000000000 ) ) ;
#10781 = DIRECTION ( 'NONE',  ( -0.8757121056631640421, -0.4828336235133042775, 0.000000000000000000 ) ) ;
#10782 = ADVANCED_FACE ( 'NONE', ( #18871 ), #17146, .F. ) ;
#10783 = DIRECTION ( 'NONE',  ( -0.000000000000000000, -0.000000000000000000, -1.000000000000000000 ) ) ;
#10784 = CARTESIAN_POINT ( 'NONE',  ( 73.12522638709218370, 7.562528597612068045E-15, 0.000000000000000000 ) ) ;
#10785 = DIRECTION ( 'NONE',  ( 0.000000000000000000, 0.000000000000000000, 1.000000000000000000 ) ) ;
#10786 = EDGE_CURVE ( 'NONE', #12366, #14475, #12101, .T. ) ;
#10787 = ORIENTED_EDGE ( 'NONE', *, *, #139, .F. ) ;
#10788 = CARTESIAN_POINT ( 'NONE',  ( -8.680847955710813579, -2.820578480814258437, 9.733165578109186811 ) ) ;
#10789 = VERTEX_POINT ( 'NONE', #8107 ) ;
#10790 = EDGE_CURVE ( 'NONE', #13492, #8141, #8978, .T. ) ;
#10791 = ADVANCED_FACE ( 'NONE', ( #9804 ), #15209, .F. ) ;
#10792 = PRODUCT_DEFINITION_SHAPE ( 'NONE', 'NONE',  #24103 ) ;
#10793 = DIRECTION ( 'NONE',  ( 0.9292670476541347035, 0.3694086546687400663, 5.551115123125782702E-17 ) ) ;
#10794 = FACE_OUTER_BOUND ( 'NONE', #9341, .T. ) ;
#10795 = ORIENTED_EDGE ( 'NONE', *, *, #6926, .F. ) ;
#10796 = ORIENTED_EDGE ( 'NONE', *, *, #10865, .T. ) ;
#10797 = DIRECTION ( 'NONE',  ( -0.000000000000000000, -1.000000000000000000, -0.000000000000000000 ) ) ;
#10798 = CARTESIAN_POINT ( 'NONE',  ( 2.935661446562616295, -9.035036904803758873, -3.659589141758142983 ) ) ;
#10799 = AXIS2_PLACEMENT_3D ( 'NONE', #300, #11490, #18963 ) ;
#10800 = CYLINDRICAL_SURFACE ( 'NONE', #14557, 5.000000000000000888 ) ;
#10801 = CARTESIAN_POINT ( 'NONE',  ( 6.250000000000000000, -10.82531754730548279, -2.500000000000000000 ) ) ;
#10802 = DIRECTION ( 'NONE',  ( -1.000000000000000000, 0.000000000000000000, 0.000000000000000000 ) ) ;
#10803 = AXIS2_PLACEMENT_3D ( 'NONE', #23657, #12508, #7032 ) ;
#10804 = DIRECTION ( 'NONE',  ( -0.000000000000000000, -0.000000000000000000, 1.000000000000000000 ) ) ;
#10805 = ORIENTED_EDGE ( 'NONE', *, *, #16810, .F. ) ;
#10806 = CARTESIAN_POINT ( 'NONE',  ( -1.029124893018731811E-15, 45.00000000000000000, 22.79827876194487857 ) ) ;
#10807 = DIRECTION ( 'NONE',  ( -1.000000000000000000, -0.000000000000000000, -0.000000000000000000 ) ) ;
#10808 = EDGE_LOOP ( 'NONE', ( #9296, #12608, #22763, #1895, #868 ) ) ;
#10809 = DIRECTION ( 'NONE',  ( 1.000000000000000000, 0.000000000000000000, 0.000000000000000000 ) ) ;
#10810 = DIRECTION ( 'NONE',  ( 1.000000000000000000, 0.000000000000000000, 0.000000000000000000 ) ) ;
#10811 = CARTESIAN_POINT ( 'NONE',  ( 5.000000000000000000, 0.000000000000000000, 0.000000000000000000 ) ) ;
#10812 = EDGE_CURVE ( 'NONE', #10731, #19902, #10928, .T. ) ;
#10813 = CARTESIAN_POINT ( 'NONE',  ( 78.94340820527399671, 7.562528597612068045E-15, 0.000000000000000000 ) ) ;
#10814 = VERTEX_POINT ( 'NONE', #6181 ) ;
#10815 = CARTESIAN_POINT ( 'NONE',  ( 10.40000000000000036, 6.613092715395708453E-16, 5.400000000000001243 ) ) ;
#10816 = FACE_OUTER_BOUND ( 'NONE', #17110, .T. ) ;
#10817 = ORIENTED_EDGE ( 'NONE', *, *, #19994, .T. ) ;
#10818 = EDGE_LOOP ( 'NONE', ( #15549, #6564, #20550, #4957, #5136, #259 ) ) ;
#10819 = CARTESIAN_POINT ( 'NONE',  ( 6.809999908187194197E-13, -9.988891130263535700, 8.706742014460230550 ) ) ;
#10820 = CARTESIAN_POINT ( 'NONE',  ( 2.935661446562616295, -9.035036904803758873, 8.806742014460233747 ) ) ;
#10821 = ADVANCED_FACE ( 'NONE', ( #15307 ), #21183, .F. ) ;
#10822 = VERTEX_POINT ( 'NONE', #19002 ) ;
#10823 = EDGE_CURVE ( 'NONE', #8265, #5826, #17404, .T. ) ;
#10824 = VECTOR ( 'NONE', #20945, 1000.000000000000000 ) ;
#10825 = EDGE_LOOP ( 'NONE', ( #18041, #19997 ) ) ;
#10826 = VECTOR ( 'NONE', #14914, 1000.000000000000000 ) ;
#10827 = DIRECTION ( 'NONE',  ( 1.000000000000000000, 0.000000000000000000, 0.000000000000000000 ) ) ;
#10828 = LINE ( 'NONE', #10716, #1040 ) ;
#10829 = LINE ( 'NONE', #20137, #12967 ) ;
#10830 = CARTESIAN_POINT ( 'NONE',  ( -2.024999999999999911, 45.00000000000000000, 27.00000000000000000 ) ) ;
#10831 = LINE ( 'NONE', #3646, #8663 ) ;
#10832 = VERTEX_POINT ( 'NONE', #13618 ) ;
#10833 = LINE ( 'NONE', #5607, #17334 ) ;
#10834 = ORIENTED_EDGE ( 'NONE', *, *, #4738, .T. ) ;
#10835 = SURFACE_STYLE_FILL_AREA ( #10943 ) ;
#10836 = CARTESIAN_POINT ( 'NONE',  ( 9.500000000000000000, 6.470877716354879437E-13, 10.05958914175814378 ) ) ;
#10837 = CARTESIAN_POINT ( 'NONE',  ( -7.543350946223124076, 5.782987462899389364, -3.500723002159527919 ) ) ;
#10838 = CARTESIAN_POINT ( 'NONE',  ( -5.799656021750657521E-13, 8.953898637140671468, -3.324357723559535849 ) ) ;
#10839 = AXIS2_PLACEMENT_3D ( 'NONE', #17592, #12227, #23241 ) ;
#10840 = DIRECTION ( 'NONE',  ( 1.000000000000000000, 0.000000000000000000, 0.000000000000000000 ) ) ;
#10841 = CARTESIAN_POINT ( 'NONE',  ( -27.70933665152130843, -40.41277845351217479, 12.00000000000000000 ) ) ;
#10843 = MANIFOLD_SOLID_BREP ( '\X2\00d8\X0\2.0mm Dowel Hole1', #7353 ) ;
#10842 = ORIENTED_EDGE ( 'NONE', *, *, #17214, .F. ) ;
#10844 = DIRECTION ( 'NONE',  ( -1.000000000000000000, 0.000000000000000000, 0.000000000000000000 ) ) ;
#10845 = ORIENTED_EDGE ( 'NONE', *, *, #9462, .T. ) ;
#10846 = CARTESIAN_POINT ( 'NONE',  ( 29.00000000000000000, 29.50000000000000355, 11.50000000000000000 ) ) ;
#10847 = CARTESIAN_POINT ( 'NONE',  ( 2.454813078130514813E-15, 16.67999999999999972, 12.00000000000000000 ) ) ;
#10848 = EDGE_CURVE ( 'NONE', #3277, #17283, #13241, .T. ) ;
#10849 = EDGE_LOOP ( 'NONE', ( #14000, #7483, #16350, #12107 ) ) ;
#10850 = FACE_OUTER_BOUND ( 'NONE', #22407, .T. ) ;
#10851 = CARTESIAN_POINT ( 'NONE',  ( 29.00000000000000000, -29.50000000000000355, 12.00000000000000000 ) ) ;
#10852 = DIRECTION ( 'NONE',  ( 0.000000000000000000, 0.000000000000000000, 1.000000000000000000 ) ) ;
#10853 = DIRECTION ( 'NONE',  ( 0.000000000000000000, 0.000000000000000000, 1.000000000000000000 ) ) ;
#10854 = ORIENTED_EDGE ( 'NONE', *, *, #21368, .F. ) ;
#10855 = CYLINDRICAL_SURFACE ( 'NONE', #6072, 23.85000000000000497 ) ;
#10856 = CARTESIAN_POINT ( 'NONE',  ( 5.871322893123449127, 8.081182679344781405, -10.35958914175814627 ) ) ;
#10857 = ORIENTED_EDGE ( 'NONE', *, *, #24057, .T. ) ;
#10858 = ORIENTED_EDGE ( 'NONE', *, *, #2974, .T. ) ;
#10859 = LINE ( 'NONE', #12575, #20052 ) ;
#10860 = CARTESIAN_POINT ( 'NONE',  ( 79.23840997654417606, -9.244463733058732095E-30, 5.000000000000007994 ) ) ;
#10861 = EDGE_CURVE ( 'NONE', #18771, #13485, #13503, .T. ) ;
#10862 = EDGE_CURVE ( 'NONE', #6922, #21416, #4115, .T. ) ;
#10863 = EDGE_LOOP ( 'NONE', ( #316, #7169, #12629, #7401, #21308 ) ) ;
#10864 = CARTESIAN_POINT ( 'NONE',  ( -28.99999999999999645, 29.50000000000000000, 27.00000000000000000 ) ) ;
#10865 = EDGE_CURVE ( 'NONE', #23486, #8523, #17986, .T. ) ;
#10866 = FACE_OUTER_BOUND ( 'NONE', #6526, .T. ) ;
#10867 = VERTEX_POINT ( 'NONE', #4849 ) ;
#10868 =( REPRESENTATION_RELATIONSHIP ('NONE','NONE', #21748, #2851 ) REPRESENTATION_RELATIONSHIP_WITH_TRANSFORMATION ( #11119 )SHAPE_REPRESENTATION_RELATIONSHIP( ) );
#10869 = LINE ( 'NONE', #17869, #23553 ) ;
#10870 = EDGE_CURVE ( 'NONE', #2976, #15317, #5074, .T. ) ;
#10871 = DIRECTION ( 'NONE',  ( 0.8571673007021120005, 1.049727191138618326E-16, -0.5150380749100547106 ) ) ;
#10872 = PLANE ( 'NONE',  #2969 ) ;
#10873 = CARTESIAN_POINT ( 'NONE',  ( 8.000000000000000000, 0.000000000000000000, 12.50000000000000000 ) ) ;
#10874 = EDGE_LOOP ( 'NONE', ( #16673, #17245 ) ) ;
#10875 = AXIS2_PLACEMENT_3D ( 'NONE', #3487, #21917, #6678 ) ;
#10877 = ORIENTED_EDGE ( 'NONE', *, *, #20547, .F. ) ;
#10876 = VECTOR ( 'NONE', #936, 1000.000000000000000 ) ;
#10878 = ORIENTED_EDGE ( 'NONE', *, *, #16508, .T. ) ;
#10879 = CARTESIAN_POINT ( 'NONE',  ( 83.30704456891035647, 5.000000000000015099, 0.000000000000000000 ) ) ;
#10880 = CARTESIAN_POINT ( 'NONE',  ( 85.05659179472598908, 7.420530141404717394E-15, 0.000000000000000000 ) ) ;
#10881 = EDGE_LOOP ( 'NONE', ( #12478, #17128, #6517, #20473 ) ) ;
#10882 = CARTESIAN_POINT ( 'NONE',  ( 65.27272727272728048, 7.491529369508391930E-15, 0.000000000000000000 ) ) ;
#10883 = EDGE_LOOP ( 'NONE', ( #12657, #13766, #23500, #21408 ) ) ;
#10884 = CARTESIAN_POINT ( 'NONE',  ( 5.000000000000000000, 2.342598717236902939, -4.057500000000001883 ) ) ;
#10885 = DIRECTION ( 'NONE',  ( 0.000000000000000000, -0.000000000000000000, -1.000000000000000000 ) ) ;
#10886 = B_SPLINE_CURVE_WITH_KNOTS ( 'NONE', 3,
 ( #19537, #2813, #17700, #15876 ),
 .UNSPECIFIED., .F., .F.,
 ( 4, 4 ),
 ( 3.940689367451708065E-16, 0.001795700496623581352 ),
 .UNSPECIFIED. ) ;
#10887 = ADVANCED_FACE ( 'NONE', ( #17774 ), #21679, .T. ) ;
#10888 = ADVANCED_FACE ( 'NONE', ( #19735 ), #3014, .F. ) ;
#10889 = DIRECTION ( 'NONE',  ( 1.000000000000000000, 0.000000000000000000, 0.000000000000000000 ) ) ;
#10890 = DIRECTION ( 'NONE',  ( -0.000000000000000000, -0.000000000000000000, -1.000000000000000000 ) ) ;
#10891 = DIRECTION ( 'NONE',  ( -0.000000000000000000, -0.000000000000000000, -1.000000000000000000 ) ) ;
#10892 = DIRECTION ( 'NONE',  ( 1.000000000000000000, 1.360567432138674546E-16, -0.000000000000000000 ) ) ;
#10893 = CIRCLE ( 'NONE', #16737, 4.499999999999997335 ) ;
#10894 = DIRECTION ( 'NONE',  ( -1.000000000000000000, 0.000000000000000000, 0.000000000000000000 ) ) ;
#10895 = DIRECTION ( 'NONE',  ( 0.000000000000000000, 0.000000000000000000, 1.000000000000000000 ) ) ;
#10896 = CARTESIAN_POINT ( 'NONE',  ( 0.000000000000000000, 12.00453763395396756, -7.608955687739546114 ) ) ;
#10897 = CARTESIAN_POINT ( 'NONE',  ( 2.682529543900284974, -8.255977015246234174, 8.233165578109190363 ) ) ;
#10898 = ORIENTED_EDGE ( 'NONE', *, *, #18486, .T. ) ;
#10899 = SHAPE_DEFINITION_REPRESENTATION ( #15021, #15960 ) ;
#10900 = LINE ( 'NONE', #18367, #3453 ) ;
#10901 = ORIENTED_EDGE ( 'NONE', *, *, #6153, .T. ) ;
#10902 = EDGE_LOOP ( 'NONE', ( #12088, #4615, #7800, #14162 ) ) ;
#10903 = CARTESIAN_POINT ( 'NONE',  ( 23.84999999999999432, -15.03999999999999559, 25.00000000000000000 ) ) ;
#10904 = CARTESIAN_POINT ( 'NONE',  ( -5.871322893123450015, -8.081182679344781405, -7.359589141758143604 ) ) ;
#10905 = EDGE_CURVE ( 'NONE', #17223, #5066, #3010, .T. ) ;
#10906 = CIRCLE ( 'NONE', #418, 1.500000000000001332 ) ;
#10907 = FACE_OUTER_BOUND ( 'NONE', #22700, .T. ) ;
#10908 = CARTESIAN_POINT ( 'NONE',  ( 6.250000000000000000, -10.82531754730548279, -2.500000000000000000 ) ) ;
#10909 = DIRECTION ( 'NONE',  ( 1.000000000000000000, 1.224606353822377258E-16, 0.000000000000000000 ) ) ;
#10910 = ADVANCED_FACE ( 'NONE', ( #17893 ), #23829, .F. ) ;
#10911 = CARTESIAN_POINT ( 'NONE',  ( 0.000000000000000000, 0.000000000000000000, 0.000000000000000000 ) ) ;
#10912 = EDGE_CURVE ( 'NONE', #11339, #16085, #19954, .T. ) ;
#10913 = EDGE_CURVE ( 'NONE', #4215, #19427, #937, .T. ) ;
#10914 = CARTESIAN_POINT ( 'NONE',  ( 23.85000000000000497, 15.03999999999999915, 25.00000000000000000 ) ) ;
#10915 = DIRECTION ( 'NONE',  ( -1.000000000000000000, -2.600433232233976523E-16, 0.000000000000000000 ) ) ;
#10916 = DIRECTION ( 'NONE',  ( 0.000000000000000000, 0.000000000000000000, 1.000000000000000000 ) ) ;
#10917 = CARTESIAN_POINT ( 'NONE',  ( 17.32314925601269451, 8.733074366907754182, -3.769949228126190377 ) ) ;
#10918 = DIRECTION ( 'NONE',  ( 0.5579568342432823513, 0.8298699724180977899, 0.000000000000000000 ) ) ;
#10919 = DIRECTION ( 'NONE',  ( -0.000000000000000000, 0.000000000000000000, -1.000000000000000000 ) ) ;
#10920 = CARTESIAN_POINT ( 'NONE',  ( -5.871322893123450015, -8.081182679344781405, -10.50674201446023304 ) ) ;
#10921 = ORIENTED_EDGE ( 'NONE', *, *, #16821, .F. ) ;
#10922 = ORIENTED_EDGE ( 'NONE', *, *, #15110, .T. ) ;
#10923=STYLED_ITEM('',(#24141),#18364);
#10924 = CARTESIAN_POINT ( 'NONE',  ( -9.500000000000000000, -6.482511860946779655E-13, 10.20674201446023233 ) ) ;
#10925 = CARTESIAN_POINT ( 'NONE',  ( 7.685661446562381371, -5.583959896777971110, 5.006742014460233037 ) ) ;
#10926 = DIRECTION ( 'NONE',  ( 0.000000000000000000, 0.000000000000000000, 1.000000000000000000 ) ) ;
#10927 = VERTEX_POINT ( 'NONE', #18004 ) ;
#10928 = CIRCLE ( 'NONE', #5499, 5.000000000000007994 ) ;
#10929 = ORIENTED_EDGE ( 'NONE', *, *, #20212, .F. ) ;
#10930 =( NAMED_UNIT ( * ) PLANE_ANGLE_UNIT ( ) SI_UNIT ( $, .RADIAN. ) );
#10931 = DIRECTION ( 'NONE',  ( 0.000000000000000000, 0.000000000000000000, 1.000000000000000000 ) ) ;
#10932 = CARTESIAN_POINT ( 'NONE',  ( 23.00000000000000000, 0.000000000000000000, 0.000000000000000000 ) ) ;
#10933 = DIRECTION ( 'NONE',  ( 0.000000000000000000, 0.000000000000000000, -1.000000000000000000 ) ) ;
#10934 = EDGE_CURVE ( 'NONE', #8356, #23464, #23279, .T. ) ;
#10935 = DIRECTION ( 'NONE',  ( 0.000000000000000000, 0.000000000000000000, 1.000000000000000000 ) ) ;
#10936 =( LENGTH_UNIT ( ) NAMED_UNIT ( * ) SI_UNIT ( .MILLI., .METRE. ) );
#10937 = LINE ( 'NONE', #24098, #17228 ) ;
#10938 = ORIENTED_EDGE ( 'NONE', *, *, #16506, .T. ) ;
#10939 = CIRCLE ( 'NONE', #19928, 5.000000000000007994 ) ;
#10940 = EDGE_CURVE ( 'NONE', #17886, #10927, #12011, .T. ) ;
#10941 = DIRECTION ( 'NONE',  ( 0.000000000000000000, 0.000000000000000000, 1.000000000000000000 ) ) ;
#10942 = EDGE_CURVE ( 'NONE', #13312, #12511, #16036, .T. ) ;
#10943 = FILL_AREA_STYLE ('',( #7063 ) ) ;
#10944 = DIRECTION ( 'NONE',  ( -1.000000000000000000, -0.000000000000000000, -0.000000000000000000 ) ) ;
#10945 = CIRCLE ( 'NONE', #81, 4.999999999999997335 ) ;
#10946 = DIRECTION ( 'NONE',  ( 0.000000000000000000, 0.000000000000000000, 1.000000000000000000 ) ) ;
#10947 = DIRECTION ( 'NONE',  ( 0.000000000000000000, 0.000000000000000000, 1.000000000000000000 ) ) ;
#10948 = DIRECTION ( 'NONE',  ( 0.000000000000000000, 0.000000000000000000, 1.000000000000000000 ) ) ;
#10949 = CARTESIAN_POINT ( 'NONE',  ( -28.99999999999999645, -29.50000000000000000, -3.000000000000000000 ) ) ;
#10950 = ORIENTED_EDGE ( 'NONE', *, *, #7503, .F. ) ;
#10951 = CARTESIAN_POINT ( 'NONE',  ( 90.00000000000000000, 5.109226446042757607E-16, -4.171999999999999709 ) ) ;
#10952 = ORIENTED_EDGE ( 'NONE', *, *, #12393, .F. ) ;
#10953 = CARTESIAN_POINT ( 'NONE',  ( 71.67068093254673045, 7.562528597612068045E-15, 0.000000000000000000 ) ) ;
#10954 = VERTEX_POINT ( 'NONE', #4723 ) ;
#10955 = CARTESIAN_POINT ( 'NONE',  ( 42.62132034355962418, -25.48082444701818616, 6.173874856195240421E-16 ) ) ;
#10956 = CARTESIAN_POINT ( 'NONE',  ( 23.00000000000000000, 14.21257171757157245, 6.139082186136624486 ) ) ;
#10957 = CARTESIAN_POINT ( 'NONE',  ( 84.76159002345582394, 6.123233995736675563E-16, -5.000000000000007994 ) ) ;
#10958 = VECTOR ( 'NONE', #18661, 1000.000000000000000 ) ;
#10959 = AXIS2_PLACEMENT_3D ( 'NONE', #18635, #11398, #18873 ) ;
#10960 = CIRCLE ( 'NONE', #9025, 1.000000000000000222 ) ;
#10961 = DIRECTION ( 'NONE',  ( -1.000000000000000000, -0.000000000000000000, -0.000000000000000000 ) ) ;
#10962 = EDGE_CURVE ( 'NONE', #20443, #18942, #21105, .T. ) ;
#10963 = CARTESIAN_POINT ( 'NONE',  ( -5.871322893123450015, -8.081182679344781405, -7.359589141758143604 ) ) ;
#10964 = VERTEX_POINT ( 'NONE', #19603 ) ;
#10965 = EDGE_LOOP ( 'NONE', ( #7699, #18181 ) ) ;
#10966 = DIRECTION ( 'NONE',  ( -0.000000000000000000, 1.000000000000000000, -0.000000000000000000 ) ) ;
#10967 = DIRECTION ( 'NONE',  ( 0.000000000000000000, -0.000000000000000000, 1.000000000000000000 ) ) ;
#10968 = EDGE_CURVE ( 'NONE', #21802, #8229, #10945, .T. ) ;
#10969 = DIRECTION ( 'NONE',  ( 0.000000000000000000, -1.000000000000000000, 0.000000000000000000 ) ) ;
#10970 = CIRCLE ( 'NONE', #22298, 1.000000000000000888 ) ;
#10971 = VECTOR ( 'NONE', #11334, 1000.000000000000000 ) ;
#10972 = ORIENTED_EDGE ( 'NONE', *, *, #21052, .F. ) ;
#10973 = CIRCLE ( 'NONE', #22320, 10.94716442891539465 ) ;
#10974 = DIRECTION ( 'NONE',  ( -0.000000000000000000, 0.000000000000000000, 1.000000000000000000 ) ) ;
#10975 = VECTOR ( 'NONE', #24027, 1000.000000000000000 ) ;
#10976 = AXIS2_PLACEMENT_3D ( 'NONE', #11725, #21283, #19201 ) ;
#10977 = CARTESIAN_POINT ( 'NONE',  ( 76.32931906745326955, 7.420530141404717394E-15, 0.000000000000000000 ) ) ;
#10978 = ORIENTED_EDGE ( 'NONE', *, *, #2097, .T. ) ;
#10979 = VECTOR ( 'NONE', #13073, 1000.000000000000000 ) ;
#10980 = DIRECTION ( 'NONE',  ( 0.7052211081716905916, -0.7089874389501501506, -0.000000000000000000 ) ) ;
#10981 = DIRECTION ( 'NONE',  ( -0.000000000000000000, -0.000000000000000000, -1.000000000000000000 ) ) ;
#10982 = DIRECTION ( 'NONE',  ( 0.000000000000000000, 0.000000000000000000, 1.000000000000000000 ) ) ;
#10983 = CARTESIAN_POINT ( 'NONE',  ( 61.78386452199871570, 6.123233995736675563E-16, -5.000000000000007994 ) ) ;
#10984 = ORIENTED_EDGE ( 'NONE', *, *, #21227, .F. ) ;
#10985 = ADVANCED_FACE ( 'NONE', ( #2882 ), #456, .T. ) ;
#10986 = EDGE_LOOP ( 'NONE', ( #18299, #8222, #18728, #22021 ) ) ;
#10987 = CIRCLE ( 'NONE', #12178, 17.87500000001787726 ) ;
#10988 = EDGE_CURVE ( 'NONE', #128, #2676, #8224, .T. ) ;
#10989 = EDGE_LOOP ( 'NONE', ( #7638, #11181, #19852, #23262 ) ) ;
#10991 = CIRCLE ( 'NONE', #10608, 18.50000000000000000 ) ;
#10990 = CARTESIAN_POINT ( 'NONE',  ( -31.74999999999995737, 0.000000000000000000, 0.000000000000000000 ) ) ;
#10992 = AXIS2_PLACEMENT_3D ( 'NONE', #15806, #8585, #4713 ) ;
#10993 = VECTOR ( 'NONE', #297, 999.9999999999998863 ) ;
#10994 = AXIS2_PLACEMENT_3D ( 'NONE', #18333, #7439, #7229 ) ;
#10995 = CARTESIAN_POINT ( 'NONE',  ( 4.489900896931573904, 0.000000000000000000, 0.000000000000000000 ) ) ;
#10996 = VERTEX_POINT ( 'NONE', #9198 ) ;
#10997 = CARTESIAN_POINT ( 'NONE',  ( -40.29291594121673370, 26.62062637246459929, 11.00000000000000000 ) ) ;
#10998 = EDGE_CURVE ( 'NONE', #21352, #411, #7361, .T. ) ;
#10999 = EDGE_CURVE ( 'NONE', #5168, #19859, #17192, .T. ) ;
#11000 = CARTESIAN_POINT ( 'NONE',  ( -20.85000000000000853, 15.04000000000000092, 27.00000000000000000 ) ) ;
#11001 = VECTOR ( 'NONE', #9927, 1000.000000000000000 ) ;
#11002 = ORIENTED_EDGE ( 'NONE', *, *, #13116, .T. ) ;
#11003 = DIRECTION ( 'NONE',  ( 0.000000000000000000, -1.000000000000000000, 0.000000000000000000 ) ) ;
#11004 = CARTESIAN_POINT ( 'NONE',  ( 42.00000000000000000, 25.22443390181681266, -0.6213203435596420521 ) ) ;
#11005 = CARTESIAN_POINT ( 'NONE',  ( 23.00000000000000000, 6.242160243097294448, -9.879763041175060323 ) ) ;
#11006 = DIRECTION ( 'NONE',  ( 0.000000000000000000, 0.000000000000000000, -1.000000000000000000 ) ) ;
#11007 = CARTESIAN_POINT ( 'NONE',  ( 84.76159002345582394, 7.562528597612068045E-15, 0.000000000000000000 ) ) ;
#11008 = CARTESIAN_POINT ( 'NONE',  ( 65.85249911436491743, 7.562528597612068045E-15, 0.000000000000000000 ) ) ;
#11009 = CIRCLE ( 'NONE', #8679, 5.000000000000007994 ) ;
#11010 = DIRECTION ( 'NONE',  ( -1.000000000000000000, 0.000000000000000000, 0.000000000000000000 ) ) ;
#11011 = LINE ( 'NONE', #15046, #23922 ) ;
#11012 = CIRCLE ( 'NONE', #917, 0.9599481167642566204 ) ;
#11013 = CARTESIAN_POINT ( 'NONE',  ( 0.000000000000000000, 2.342598717236913153, 4.057500000000004547 ) ) ;
#11014 = AXIS2_PLACEMENT_3D ( 'NONE', #6639, #21522, #12234 ) ;
#11015 = AXIS2_PLACEMENT_3D ( 'NONE', #10815, #8877, #23888 ) ;
#11016 = ORIENTED_EDGE ( 'NONE', *, *, #22861, .F. ) ;
#11017 = CARTESIAN_POINT ( 'NONE',  ( 8.680847955711199049, -2.820578480813074496, 12.53316557810918752 ) ) ;
#11018 = ORIENTED_EDGE ( 'NONE', *, *, #22246, .T. ) ;
#11019 = AXIS2_PLACEMENT_3D ( 'NONE', #9520, #9170, #20538 ) ;
#11020 = ADVANCED_FACE ( 'NONE', ( #7256 ), #1769, .F. ) ;
#11021 = AXIS2_PLACEMENT_3D ( 'NONE', #4511, #4370, #9600 ) ;
#11022 = PRODUCT_CONTEXT ( 'NONE', #17740, 'mechanical' ) ;
#11023 = CYLINDRICAL_SURFACE ( 'NONE', #10097, 1.000000000000002442 ) ;
#11024 = ORIENTED_EDGE ( 'NONE', *, *, #1160, .T. ) ;
#11025 = ORIENTED_EDGE ( 'NONE', *, *, #20214, .T. ) ;
#11026 = EDGE_CURVE ( 'NONE', #192, #8001, #14091, .T. ) ;
#11027 = CARTESIAN_POINT ( 'NONE',  ( -8.790499351057960098, 3.504513977298572946, -12.05035160442407971 ) ) ;
#11028 = CARTESIAN_POINT ( 'NONE',  ( 8.680847955711199049, -2.820578480813074496, -8.533165578109187521 ) ) ;
#11029 = ADVANCED_FACE ( 'NONE', ( #24084 ), #1646, .T. ) ;
#11030 = ORIENTED_EDGE ( 'NONE', *, *, #13568, .F. ) ;
#11031 = CARTESIAN_POINT ( 'NONE',  ( 23.85000000000000497, 15.03999999999999915, 27.00000000000000000 ) ) ;
#11032 = DIRECTION ( 'NONE',  ( -0.000000000000000000, -0.000000000000000000, -1.000000000000000000 ) ) ;
#11033 = CARTESIAN_POINT ( 'NONE',  ( 0.000000000000000000, -15.03999999999999737, 2.200000000000000178 ) ) ;
#11034 = CIRCLE ( 'NONE', #223, 5.000000000000007994 ) ;
#11035 = CYLINDRICAL_SURFACE ( 'NONE', #11582, 10.00000000000000178 ) ;
#11036 = DIRECTION ( 'NONE',  ( -0.000000000000000000, -0.000000000000000000, -1.000000000000000000 ) ) ;
#11037 = AXIS2_PLACEMENT_3D ( 'NONE', #8834, #16272, #12370 ) ;
#11038 = AXIS2_PLACEMENT_3D ( 'NONE', #23373, #4826, #13703 ) ;
#11039 = DIRECTION ( 'NONE',  ( 4.613626265895764052E-16, 1.000000000000000000, -0.000000000000000000 ) ) ;
#11040 = DIRECTION ( 'NONE',  ( -1.000000000000000000, -1.224606353822377258E-16, -0.000000000000000000 ) ) ;
#11041 = AXIS2_PLACEMENT_3D ( 'NONE', #6053, #7982, #9570 ) ;
#11042 = CARTESIAN_POINT ( 'NONE',  ( -30.44534269664590198, 40.40463133211079594, 27.00000000000000000 ) ) ;
#11043 = VECTOR ( 'NONE', #14983, 1000.000000000000000 ) ;
#11044 = FACE_OUTER_BOUND ( 'NONE', #19317, .T. ) ;
#11045 = PLANE ( 'NONE',  #16492 ) ;
#11046 = CARTESIAN_POINT ( 'NONE',  ( -7.685661446562381371, 5.583959896777970222, -10.00674201446023481 ) ) ;
#11047 = DIRECTION ( 'NONE',  ( -1.000000000000000000, -0.000000000000000000, -0.000000000000000000 ) ) ;
#11048 = ORIENTED_EDGE ( 'NONE', *, *, #6076, .F. ) ;
#11049 = ORIENTED_EDGE ( 'NONE', *, *, #275, .F. ) ;
#11050 = CARTESIAN_POINT ( 'NONE',  ( 2.935661446561383503, 9.035036904804158553, 11.60674201446023268 ) ) ;
#11051 = VERTEX_POINT ( 'NONE', #20199 ) ;
#11052 = ORIENTED_EDGE ( 'NONE', *, *, #18592, .F. ) ;
#11053 = AXIS2_PLACEMENT_3D ( 'NONE', #21844, #16341, #23691 ) ;
#11054 = VECTOR ( 'NONE', #983, 1000.000000000000000 ) ;
#11055 = EDGE_CURVE ( 'NONE', #6327, #16103, #19161, .T. ) ;
#11056 = DIRECTION ( 'NONE',  ( -1.000000000000000000, 0.000000000000000000, 0.000000000000000000 ) ) ;
#11057 = CARTESIAN_POINT ( 'NONE',  ( -2.935661446561384391, -9.035036904804158553, 9.459589141758144137 ) ) ;
#11058 = EDGE_CURVE ( 'NONE', #7243, #3370, #14799, .T. ) ;
#11059 = CIRCLE ( 'NONE', #22780, 5.000000000000007994 ) ;
#11060 = CARTESIAN_POINT ( 'NONE',  ( -20.85000000000000497, -15.03999999999999737, 2.200000000000000178 ) ) ;
#11061 = DIRECTION ( 'NONE',  ( 1.000000000000000000, 0.000000000000000000, 0.000000000000000000 ) ) ;
#11062 = DIRECTION ( 'NONE',  ( -0.000000000000000000, -0.000000000000000000, -1.000000000000000000 ) ) ;
#11063 = VERTEX_POINT ( 'NONE', #11005 ) ;
#11064 = PLANE ( 'NONE',  #452 ) ;
#11065 = CARTESIAN_POINT ( 'NONE',  ( 58.57977184163763695, 5.000000000000015987, 0.000000000000000000 ) ) ;
#11066 = DIRECTION ( 'NONE',  ( -1.000000000000000000, -1.224606353822377258E-16, -0.000000000000000000 ) ) ;
#11067 = DIRECTION ( 'NONE',  ( -0.000000000000000000, -0.000000000000000000, -1.000000000000000000 ) ) ;
#11068 = VECTOR ( 'NONE', #19287, 1000.000000000000000 ) ;
#11069 = AXIS2_PLACEMENT_3D ( 'NONE', #12974, #3950, #3589 ) ;
#11070 = LINE ( 'NONE', #3783, #20278 ) ;
#11071 = AXIS2_PLACEMENT_3D ( 'NONE', #13896, #21077, #1953 ) ;
#11072 = CARTESIAN_POINT ( 'NONE',  ( -28.99999999999999645, 29.50000000000000000, -2.224999999999995204 ) ) ;
#11073 = ORIENTED_EDGE ( 'NONE', *, *, #13289, .T. ) ;
#11074 = ADVANCED_FACE ( 'NONE', ( #20309 ), #1251, .T. ) ;
#11075 = LINE ( 'NONE', #10951, #12637 ) ;
#11076 = VECTOR ( 'NONE', #14172, 1000.000000000000000 ) ;
#11077 = ORIENTED_EDGE ( 'NONE', *, *, #18248, .T. ) ;
#11078 = DIRECTION ( 'NONE',  ( -0.000000000000000000, -0.000000000000000000, -1.000000000000000000 ) ) ;
#11079 = EDGE_LOOP ( 'NONE', ( #3604, #20414, #16382, #9594, #13460 ) ) ;
#11080 = EDGE_CURVE ( 'NONE', #3333, #14771, #18480, .T. ) ;
#11081 = AXIS2_PLACEMENT_3D ( 'NONE', #8859, #5202, #12865 ) ;
#11082 = AXIS2_PLACEMENT_3D ( 'NONE', #23035, #830, #19977 ) ;
#11083 = CARTESIAN_POINT ( 'NONE',  ( -40.66734255040736201, -26.56420859267092283, -1.500000000000000000 ) ) ;
#11084 = EDGE_CURVE ( 'NONE', #19902, #891, #11726, .T. ) ;
#11085 = CARTESIAN_POINT ( 'NONE',  ( -31.74999999999995737, 6.123233995736767268E-16, -5.000000000000000888 ) ) ;
#11086 = ADVANCED_FACE ( 'NONE', ( #20425 ), #12522, .F. ) ;
#11087 = EDGE_CURVE ( 'NONE', #9521, #14785, #11130, .T. ) ;
#11088 =( BOUNDED_CURVE ( )  B_SPLINE_CURVE ( 2, ( #21314, #4846, #6425, #17889, #16167, #8219, #23142, #12379, #12008, #19844, #6549 ),
 .UNSPECIFIED., .F., .T. ) 
 B_SPLINE_CURVE_WITH_KNOTS ( ( 3, 2, 2, 2, 2, 3 ),
 ( 0.4000000000000000222, 0.4199999999999999845, 0.4400000000000000022, 0.4600000000000000200, 0.4799999999999999822, 0.5000000000000000000 ),
 .UNSPECIFIED. ) 
 CURVE ( )  GEOMETRIC_REPRESENTATION_ITEM ( )  RATIONAL_B_SPLINE_CURVE ( ( 1.000000000000000000, 0.9510565162951535312, 1.000000000000000000, 0.9510565162951535312, 1.000000000000000000, 0.9510565162951535312, 1.000000000000000000, 0.9510565162951535312, 1.000000000000000000, 0.9510565162951535312, 1.000000000000000000 ) ) 
 REPRESENTATION_ITEM ( '' )  );
#11089 = AXIS2_PLACEMENT_3D ( 'NONE', #4567, #22728, #23092 ) ;
#11090 = CARTESIAN_POINT ( 'NONE',  ( -5.871322893123450015, -8.081182679344781405, -9.359589141758146269 ) ) ;
#11091 = ORIENTED_EDGE ( 'NONE', *, *, #20894, .T. ) ;
#11092 = AXIS2_PLACEMENT_3D ( 'NONE', #21861, #7208, #3186 ) ;
#11093 = ORIENTED_EDGE ( 'NONE', *, *, #20615, .F. ) ;
#11094 = DIRECTION ( 'NONE',  ( 1.000000000000000000, 0.000000000000000000, 0.000000000000000000 ) ) ;
#11095 = DIRECTION ( 'NONE',  ( 1.000000000000000000, 0.000000000000000000, 0.000000000000000000 ) ) ;
#11096 = VECTOR ( 'NONE', #5430, 1000.000000000000000 ) ;
#11097 = ORIENTED_EDGE ( 'NONE', *, *, #10179, .F. ) ;
#11098 = DIRECTION ( 'NONE',  ( 0.000000000000000000, 0.000000000000000000, 1.000000000000000000 ) ) ;
#11099 = AXIS2_PLACEMENT_3D ( 'NONE', #20503, #17176, #7538 ) ;
#11100 = EDGE_LOOP ( 'NONE', ( #1571, #2311, #2230, #19773 ) ) ;
#11101 = CYLINDRICAL_SURFACE ( 'NONE', #21559, 15.00000000000000000 ) ;
#11102 = LINE ( 'NONE', #20055, #14552 ) ;
#11103 = ADVANCED_FACE ( 'NONE', ( #18605 ), #1884, .T. ) ;
#11104 = CARTESIAN_POINT ( 'NONE',  ( 9.999999999999998224, 1.224646799147353059E-15, 15.50000000000000000 ) ) ;
#11105 = ORIENTED_EDGE ( 'NONE', *, *, #19783, .T. ) ;
#11106 = ORIENTED_EDGE ( 'NONE', *, *, #9423, .T. ) ;
#11107 = CYLINDRICAL_SURFACE ( 'NONE', #22234, 6.050000000006051870 ) ;
#11108 = CARTESIAN_POINT ( 'NONE',  ( 11.50000000000000000, -7.812991839788663739, -16.07708877602020436 ) ) ;
#11109 = CARTESIAN_POINT ( 'NONE',  ( -9.500000000000000000, -6.482511860946779655E-13, -4.206742014460233214 ) ) ;
#11110 = AXIS2_PLACEMENT_3D ( 'NONE', #9031, #15196, #16481 ) ;
#11111 = DIRECTION ( 'NONE',  ( 0.000000000000000000, -1.000000000000000000, 0.000000000000000000 ) ) ;
#11112 = CIRCLE ( 'NONE', #19731, 9.000000000000000000 ) ;
#11113 = CARTESIAN_POINT ( 'NONE',  ( -5.365059087799947335, 7.384370330706355290, 7.333165578109188232 ) ) ;
#11114 = ORIENTED_EDGE ( 'NONE', *, *, #19778, .T. ) ;
#11115 = EDGE_CURVE ( 'NONE', #3370, #3297, #6700, .T. ) ;
#11117 = EDGE_CURVE ( 'NONE', #5371, #7332, #10327, .T. ) ;
#11116 = VECTOR ( 'NONE', #21605, 1000.000000000000000 ) ;
#11118 = ORIENTED_EDGE ( 'NONE', *, *, #17469, .F. ) ;
#11119 = ITEM_DEFINED_TRANSFORMATION ( 'NONE', 'NONE', #14652,  #17768 ) ;
#11120 = ORIENTED_EDGE ( 'NONE', *, *, #1162, .T. ) ;
#11121 = CARTESIAN_POINT ( 'NONE',  ( -9.499999999999996447, 0.000000000000000000, 0.000000000000000000 ) ) ;
#11122 = CARTESIAN_POINT ( 'NONE',  ( 2.935661446561383503, 9.035036904804158553, 9.606742014460232681 ) ) ;
#11123 = ORIENTED_EDGE ( 'NONE', *, *, #19759, .F. ) ;
#11124 = DIRECTION ( 'NONE',  ( -1.000000000000000000, -1.224606353822377258E-16, -0.000000000000000000 ) ) ;
#11125 = AXIS2_PLACEMENT_3D ( 'NONE', #11634, #19105, #6545 ) ;
#11126 = CARTESIAN_POINT ( 'NONE',  ( 30.16774287754691386, -40.66994976491903913, -3.000000000000000000 ) ) ;
#11127 = ORIENTED_EDGE ( 'NONE', *, *, #20595, .T. ) ;
#11128 = CARTESIAN_POINT ( 'NONE',  ( 79.81818181818181301, -4.172000000000000597, 0.000000000000000000 ) ) ;
#11129 = VECTOR ( 'NONE', #22500, 999.9999999999998863 ) ;
#11130 = LINE ( 'NONE', #23976, #14473 ) ;
#11131 = FACE_BOUND ( 'NONE', #7741, .T. ) ;
#11132 = FACE_OUTER_BOUND ( 'NONE', #7357, .T. ) ;
#11133 = LINE ( 'NONE', #24089, #23591 ) ;
#11134 = EDGE_LOOP ( 'NONE', ( #6250, #7435, #21783, #18424 ) ) ;
#11135 = CARTESIAN_POINT ( 'NONE',  ( -30.16774287754692807, 40.66994976491904623, -1.500000000000000000 ) ) ;
#11136 = DIRECTION ( 'NONE',  ( 0.000000000000000000, 0.000000000000000000, 1.000000000000000000 ) ) ;
#11137 = CARTESIAN_POINT ( 'NONE',  ( -14.67173559926288107, 3.179195828807836133, -8.975010320294703803 ) ) ;
#11138 = EDGE_LOOP ( 'NONE', ( #11141, #7908, #13605, #426, #10420, #10052 ) ) ;
#11139 = ORIENTED_EDGE ( 'NONE', *, *, #23637, .T. ) ;
#11140 = CARTESIAN_POINT ( 'NONE',  ( -2.682529543900285862, 8.255977015246234174, 3.233165578109188587 ) ) ;
#11141 = ORIENTED_EDGE ( 'NONE', *, *, #6444, .F. ) ;
#11142 = EDGE_CURVE ( 'NONE', #5523, #5799, #16868, .T. ) ;
#11143 = SHAPE_DEFINITION_REPRESENTATION ( #12139, #5350 ) ;
#11144 = DIRECTION ( 'NONE',  ( 0.000000000000000000, 0.000000000000000000, -1.000000000000000000 ) ) ;
#11145 = ORIENTED_EDGE ( 'NONE', *, *, #15607, .T. ) ;
#11146 = ORIENTED_EDGE ( 'NONE', *, *, #12996, .T. ) ;
#11147 = CARTESIAN_POINT ( 'NONE',  ( 1.000000000000000222, 1.224646799147353454E-16, 0.2999999999999990452 ) ) ;
#11148 = CARTESIAN_POINT ( 'NONE',  ( -7.022953521755574080, 5.102474405759713783, -9.433165578109189653 ) ) ;
#11149 = VERTEX_POINT ( 'NONE', #9661 ) ;
#11150 = DIRECTION ( 'NONE',  ( 0.000000000000000000, -0.000000000000000000, 1.000000000000000000 ) ) ;
#11151 = DIRECTION ( 'NONE',  ( -1.000000000000000000, 2.600433232233976523E-16, 0.000000000000000000 ) ) ;
#11152 = CYLINDRICAL_SURFACE ( 'NONE', #14967, 6.050000000006050982 ) ;
#11153 = CARTESIAN_POINT ( 'NONE',  ( 78.94340820527399671, -5.000000000000000000, 6.123233995736775157E-16 ) ) ;
#11154 = ORIENTED_EDGE ( 'NONE', *, *, #12904, .T. ) ;
#11155 = DIRECTION ( 'NONE',  ( 0.5735764363510424957, 0.8191520442889943521, 0.000000000000000000 ) ) ;
#11156 = VERTEX_POINT ( 'NONE', #19199 ) ;
#11157 = EDGE_CURVE ( 'NONE', #7696, #8820, #7823, .T. ) ;
#11158 = EDGE_LOOP ( 'NONE', ( #3376, #23485, #19113, #2353, #3153 ) ) ;
#11159 = DIRECTION ( 'NONE',  ( -1.000000000000000000, -1.224606353822377258E-16, -0.000000000000000000 ) ) ;
#11160 = CARTESIAN_POINT ( 'NONE',  ( 71.09090909090909349, 7.491529369508391930E-15, 0.000000000000000000 ) ) ;
#11161 = CARTESIAN_POINT ( 'NONE',  ( 64.69295543108962931, 7.420530141404717394E-15, 0.000000000000000000 ) ) ;
#11162 = DIRECTION ( 'NONE',  ( 0.000000000000000000, -1.000000000000000000, 0.000000000000000000 ) ) ;
#11163 = DIRECTION ( 'NONE',  ( 0.000000000000000000, 0.000000000000000000, -1.000000000000000000 ) ) ;
#11164 = EDGE_CURVE ( 'NONE', #7451, #2444, #22509, .T. ) ;
#11165 = LINE ( 'NONE', #449, #2069 ) ;
#11166 =( LENGTH_UNIT ( ) NAMED_UNIT ( * ) SI_UNIT ( .MILLI., .METRE. ) );
#11167 = VERTEX_POINT ( 'NONE', #5786 ) ;
#11168 = EDGE_CURVE ( 'NONE', #7020, #20664, #3966, .T. ) ;
#11169 = EDGE_LOOP ( 'NONE', ( #6681, #9849, #14787, #17692 ) ) ;
#11170 = ADVANCED_FACE ( 'NONE', ( #11493 ), #22987, .T. ) ;
#11171 = CARTESIAN_POINT ( 'NONE',  ( 5.871322893123449127, 8.081182679344781405, 11.50674201446023126 ) ) ;
#11172 = VERTEX_POINT ( 'NONE', #17000 ) ;
#11173 = VERTEX_POINT ( 'NONE', #187 ) ;
#11174 = ORIENTED_EDGE ( 'NONE', *, *, #18875, .T. ) ;
#11175 = PLANE ( 'NONE',  #2136 ) ;
#11176 = CARTESIAN_POINT ( 'NONE',  ( 59.45454545454545325, 4.172000000000015696, 5.109226446042767468E-16 ) ) ;
#11177 = FACE_OUTER_BOUND ( 'NONE', #11412, .T. ) ;
#11178 = FILL_AREA_STYLE_COLOUR ( '', #6838 ) ;
#11179 = CARTESIAN_POINT ( 'NONE',  ( 23.00000000000000000, -0.09016380984471503157, 11.68615217844040544 ) ) ;
#11180 = CARTESIAN_POINT ( 'NONE',  ( -9.500000000000000000, -6.482511860946779655E-13, -11.05958914175814556 ) ) ;
#11181 = ORIENTED_EDGE ( 'NONE', *, *, #5495, .F. ) ;
#11182 = EDGE_CURVE ( 'NONE', #20252, #14709, #12120, .T. ) ;
#11183 = CARTESIAN_POINT ( 'NONE',  ( 0.000000000000000000, 15.03999999999999915, -27.00000000000000000 ) ) ;
#11184 = CARTESIAN_POINT ( 'NONE',  ( -41.50000000000000000, 28.80990663662250739, 12.00000000000000000 ) ) ;
#11185 = DIRECTION ( 'NONE',  ( -1.000000000000000000, 0.000000000000000000, 0.000000000000000000 ) ) ;
#11186 = CARTESIAN_POINT ( 'NONE',  ( -41.00000000000000000, -3.851859888774471706E-31, 8.500000000000000000 ) ) ;
#11187 = CARTESIAN_POINT ( 'NONE',  ( 6.999999999999999112, 0.000000000000000000, 14.02592346138681201 ) ) ;
#11188 = ADVANCED_FACE ( 'NONE', ( #22743 ), #3187, .T. ) ;
#11189 = VERTEX_POINT ( 'NONE', #13463 ) ;
#11190 = ADVANCED_FACE ( 'NONE', ( #4450 ), #17111, .F. ) ;
#11191 = CARTESIAN_POINT ( 'NONE',  ( 7.022953521754877748, 5.102474405760673903, -8.833165578109190008 ) ) ;
#11192 = AXIS2_PLACEMENT_3D ( 'NONE', #5340, #3139, #1556 ) ;
#11193 = CARTESIAN_POINT ( 'NONE',  ( 0.000000000000000000, -45.00000000000000000, -3.000000000000000000 ) ) ;
#11194 = VERTEX_POINT ( 'NONE', #4317 ) ;
#11195 = DIRECTION ( 'NONE',  ( -0.000000000000000000, -0.000000000000000000, -1.000000000000000000 ) ) ;
#11196 = ORIENTED_EDGE ( 'NONE', *, *, #1313, .T. ) ;
#11197 = DIRECTION ( 'NONE',  ( -1.000000000000000000, -0.000000000000000000, -0.000000000000000000 ) ) ;
#11198 = ORIENTED_EDGE ( 'NONE', *, *, #16613, .F. ) ;
#11199 = CARTESIAN_POINT ( 'NONE',  ( -41.99999999999997158, -25.22443390181683043, -3.000000000000000000 ) ) ;
#11200 = DIRECTION ( 'NONE',  ( -0.000000000000000000, -0.000000000000000000, 1.000000000000000000 ) ) ;
#11201 = AXIS2_PLACEMENT_3D ( 'NONE', #13459, #7707, #14796 ) ;
#11202 = CARTESIAN_POINT ( 'NONE',  ( 0.000000000000000000, 45.00000000000000000, -3.000000000000000000 ) ) ;
#11203 = PRODUCT_RELATED_PRODUCT_CATEGORY ( 'part', '', ( #4982 ) ) ;
#11204 = FACE_OUTER_BOUND ( 'NONE', #9041, .T. ) ;
#11205 = VECTOR ( 'NONE', #10406, 1000.000000000000000 ) ;
#11206 = EDGE_CURVE ( 'NONE', #671, #8434, #18768, .T. ) ;
#11207 = CARTESIAN_POINT ( 'NONE',  ( 7.685661446562381371, -5.583959896777971110, -5.859589141758143604 ) ) ;
#11208 = ORIENTED_EDGE ( 'NONE', *, *, #13056, .F. ) ;
#11209 = CARTESIAN_POINT ( 'NONE',  ( 0.000000000000000000, 45.00000000000000000, -23.99999999999999645 ) ) ;
#11210 = EDGE_LOOP ( 'NONE', ( #13247, #13184, #10130, #5913 ) ) ;
#11211 = CARTESIAN_POINT ( 'NONE',  ( 0.000000000000000000, 0.000000000000000000, 5.499999999999997335 ) ) ;
#11212 = CARTESIAN_POINT ( 'NONE',  ( 67.60204634018053582, 7.420530141404717394E-15, 0.000000000000000000 ) ) ;
#11213 = ADVANCED_FACE ( 'NONE', ( #7711, #15147 ), #22616, .T. ) ;
#11214 = EDGE_CURVE ( 'NONE', #20840, #16760, #21894, .T. ) ;
#11215 = ORIENTED_EDGE ( 'NONE', *, *, #2150, .T. ) ;
#11216 = CLOSED_SHELL ( 'NONE', ( #22202, #12056, #10335, #13178, #13615, #22822, #427, #20511 ) ) ;
#11217 = EDGE_CURVE ( 'NONE', #20174, #18469, #9771, .T. ) ;
#11218 = CARTESIAN_POINT ( 'NONE',  ( -21.13207267780287069, 38.32709852940855910, 0.000000000000000000 ) ) ;
#11219 = DIRECTION ( 'NONE',  ( -0.000000000000000000, 0.000000000000000000, 1.000000000000000000 ) ) ;
#11220 = DIRECTION ( 'NONE',  ( -0.000000000000000000, -0.000000000000000000, -1.000000000000000000 ) ) ;
#11221 = VERTEX_POINT ( 'NONE', #15405 ) ;
#11222 = DIRECTION ( 'NONE',  ( -0.000000000000000000, -0.000000000000000000, -1.000000000000000000 ) ) ;
#11223 = FACE_OUTER_BOUND ( 'NONE', #5648, .T. ) ;
#11224 = DIRECTION ( 'NONE',  ( -1.000000000000000000, 0.000000000000000000, 0.000000000000000000 ) ) ;
#11225 = CONICAL_SURFACE ( 'NONE', #744, 9.000000000000001776, 0.7853981633974431720 ) ;
#11226 = ORIENTED_EDGE ( 'NONE', *, *, #16810, .T. ) ;
#11227 = VERTEX_POINT ( 'NONE', #22875 ) ;
#11228 = EDGE_LOOP ( 'NONE', ( #5024, #11934, #17560, #6408 ) ) ;
#11229 = CONTEXT_DEPENDENT_SHAPE_REPRESENTATION ( #12590, #21519 ) ;
#11230 = ORIENTED_EDGE ( 'NONE', *, *, #8674, .F. ) ;
#11231 = FACE_OUTER_BOUND ( 'NONE', #3388, .T. ) ;
#11232 = DIRECTION ( 'NONE',  ( 0.000000000000000000, -1.000000000000000000, 0.000000000000000000 ) ) ;
#11233 = EDGE_CURVE ( 'NONE', #3225, #7640, #4759, .T. ) ;
#11234 = DIRECTION ( 'NONE',  ( 1.000000000000000000, 0.000000000000000000, 0.000000000000000000 ) ) ;
#11235 = ORIENTED_EDGE ( 'NONE', *, *, #1731, .T. ) ;
#11236 = CYLINDRICAL_SURFACE ( 'NONE', #15080, 6.050000000006050982 ) ;
#11237 = ORIENTED_EDGE ( 'NONE', *, *, #20698, .F. ) ;
#11238 = VECTOR ( 'NONE', #2750, 1000.000000000000000 ) ;
#11239 = EDGE_CURVE ( 'NONE', #16728, #11408, #9009, .T. ) ;
#11240 = EDGE_CURVE ( 'NONE', #11923, #1960, #18376, .T. ) ;
#11241 = DIRECTION ( 'NONE',  ( -0.000000000000000000, -0.000000000000000000, -1.000000000000000000 ) ) ;
#11242 = LINE ( 'NONE', #12849, #8645 ) ;
#11243 = DIRECTION ( 'NONE',  ( 0.000000000000000000, 0.000000000000000000, -1.000000000000000000 ) ) ;
#11244 = DIRECTION ( 'NONE',  ( -1.000000000000000000, 0.000000000000000000, 0.000000000000000000 ) ) ;
#11245 = EDGE_LOOP ( 'NONE', ( #18844, #276, #9781, #10401, #17608, #12596, #8421, #10127, #8794, #21840, #18203, #9554, #18532, #13448, #5721, #11990, #5782, #17005, #23899, #16630, #53, #12874, #22375, #15451 ) ) ;
#11246 = ORIENTED_EDGE ( 'NONE', *, *, #8090, .T. ) ;
#11247 = DIRECTION ( 'NONE',  ( 0.000000000000000000, 0.000000000000000000, 1.000000000000000000 ) ) ;
#11248 = LINE ( 'NONE', #20432, #18056 ) ;
#11249 = CARTESIAN_POINT ( 'NONE',  ( 75.45454545454545325, -4.172000000000000597, 0.000000000000000000 ) ) ;
#11250 = ORIENTED_EDGE ( 'NONE', *, *, #13542, .T. ) ;
#11251 = CARTESIAN_POINT ( 'NONE',  ( -1.374911245008260563, 8.680847955710920161, 3.184419859656034024 ) ) ;
#11252 = EDGE_LOOP ( 'NONE', ( #9218, #14747, #20299, #8511 ) ) ;
#11253 = CIRCLE ( 'NONE', #3881, 5.000000000000007994 ) ;
#11254 = APPLICATION_PROTOCOL_DEFINITION ( 'draft international standard', 'automotive_design', 1998, #19315 ) ;
#11255 = ORIENTED_EDGE ( 'NONE', *, *, #14299, .F. ) ;
#11256 = ORIENTED_EDGE ( 'NONE', *, *, #19600, .F. ) ;
#11257 = DIRECTION ( 'NONE',  ( -1.000000000000000000, 0.000000000000000000, 0.000000000000000000 ) ) ;
#11258 = CARTESIAN_POINT ( 'NONE',  ( 5.365059087799946447, -7.384370330706356178, -10.33316557810919001 ) ) ;
#11259 = VERTEX_POINT ( 'NONE', #13834 ) ;
#11260 = CARTESIAN_POINT ( 'NONE',  ( 0.000000000000000000, -12.99147757894464306, 6.750000000000000888 ) ) ;
#11261 = CARTESIAN_POINT ( 'NONE',  ( -8.000000000000000000, 9.797174393178825657E-16, -12.50000000000000000 ) ) ;
#11262 = PLANE ( 'NONE',  #22535 ) ;
#11263 = CARTESIAN_POINT ( 'NONE',  ( 65.85249911436491743, 5.000000000000015099, 0.000000000000000000 ) ) ;
#11264 = DIRECTION ( 'NONE',  ( 0.000000000000000000, 0.000000000000000000, 1.000000000000000000 ) ) ;
#11265 = EDGE_LOOP ( 'NONE', ( #13138, #932, #3280, #4954, #18314 ) ) ;
#11266 = CIRCLE ( 'NONE', #3900, 6.050000000006050982 ) ;
#11267 = EDGE_LOOP ( 'NONE', ( #6104, #6192, #20264, #13318 ) ) ;
#11268 = FACE_OUTER_BOUND ( 'NONE', #15100, .T. ) ;
#11269 = ADVANCED_FACE ( 'NONE', ( #2614 ), #2827, .T. ) ;
#11270 = CYLINDRICAL_SURFACE ( 'NONE', #440, 6.050000000006051870 ) ;
#11271 = DIRECTION ( 'NONE',  ( -0.000000000000000000, -0.000000000000000000, -1.000000000000000000 ) ) ;
#11272 = CARTESIAN_POINT ( 'NONE',  ( 16.19099482616364583, 6.271157271432194591, -7.149633965064781549 ) ) ;
#11273 = EDGE_CURVE ( 'NONE', #4470, #11149, #1267, .T. ) ;
#11274 = PLANE ( 'NONE',  #1370 ) ;
#11275 = CARTESIAN_POINT ( 'NONE',  ( 33.99999999999998579, -1.387778780781445676E-14, 10.49999999999999822 ) ) ;
#11276 = CARTESIAN_POINT ( 'NONE',  ( -2.935661446561384391, -9.035036904804158553, 8.606742014460234458 ) ) ;
#11277 = ORIENTED_EDGE ( 'NONE', *, *, #18683, .T. ) ;
#11278 = ORIENTED_EDGE ( 'NONE', *, *, #14374, .T. ) ;
#11279 = ORIENTED_EDGE ( 'NONE', *, *, #2757, .T. ) ;
#11280 = ORIENTED_EDGE ( 'NONE', *, *, #9348, .F. ) ;
#11281 =( NAMED_UNIT ( * ) SI_UNIT ( $, .STERADIAN. ) SOLID_ANGLE_UNIT ( ) );
#11282 = DIRECTION ( 'NONE',  ( 1.000000000000000000, 0.000000000000000000, 0.000000000000000000 ) ) ;
#11283 = AXIS2_PLACEMENT_3D ( 'NONE', #15500, #17712, #10121 ) ;
#11284 = CIRCLE ( 'NONE', #809, 1.000000000000000222 ) ;
#11285 = DIRECTION ( 'NONE',  ( 0.000000000000000000, 0.000000000000000000, 1.000000000000000000 ) ) ;
#11286 = EDGE_CURVE ( 'NONE', #18239, #16829, #8644, .T. ) ;
#11287 = DIRECTION ( 'NONE',  ( 1.000000000000000000, 0.000000000000000000, 0.000000000000000000 ) ) ;
#11288 = DIRECTION ( 'NONE',  ( -1.000000000000000000, -0.000000000000000000, -0.000000000000000000 ) ) ;
#11289 = SURFACE_SIDE_STYLE ('',( #3772 ) ) ;
#11290 = CYLINDRICAL_SURFACE ( 'NONE', #21956, 1.000000000000000888 ) ;
#11291 = EDGE_CURVE ( 'NONE', #16095, #1231, #12540, .T. ) ;
#11292 = CARTESIAN_POINT ( 'NONE',  ( -28.99999999999999645, 29.50000000000000000, 27.00000000000000000 ) ) ;
#11293 = EDGE_LOOP ( 'NONE', ( #20244, #17934 ) ) ;
#11294 = EDGE_CURVE ( 'NONE', #8124, #6155, #22304, .T. ) ;
#11295 = LINE ( 'NONE', #4009, #12665 ) ;
#11296 = FILL_AREA_STYLE_COLOUR ( '', #12517 ) ;
#11297 = EDGE_CURVE ( 'NONE', #21740, #1756, #21521, .T. ) ;
#11298 = CARTESIAN_POINT ( 'NONE',  ( 20.85000000000000853, 15.03999999999999915, -25.00000000000000000 ) ) ;
#11299 = CARTESIAN_POINT ( 'NONE',  ( 86.51113724927145654, 7.420530141404717394E-15, 0.000000000000000000 ) ) ;
#11300 =( GEOMETRIC_REPRESENTATION_CONTEXT ( 3 ) GLOBAL_UNCERTAINTY_ASSIGNED_CONTEXT ( ( #13754 ) ) GLOBAL_UNIT_ASSIGNED_CONTEXT ( ( #11770, #104, #5820 ) ) REPRESENTATION_CONTEXT ( 'NONE', 'WORKASPACE' ) );
#11301 = DIRECTION ( 'NONE',  ( -0.000000000000000000, -0.000000000000000000, -1.000000000000000000 ) ) ;
#11302 = PRODUCT_DEFINITION_SHAPE ( 'NONE', 'NONE',  #8534 ) ;
#11303 = VERTEX_POINT ( 'NONE', #21403 ) ;
#11304 = FACE_OUTER_BOUND ( 'NONE', #1003, .T. ) ;
#11305 = ORIENTED_EDGE ( 'NONE', *, *, #14374, .F. ) ;
#11306 = CARTESIAN_POINT ( 'NONE',  ( 3.890962118697714531E-15, 15.50000000000000000, -2.999999999999999112 ) ) ;
#11307 = ORIENTED_EDGE ( 'NONE', *, *, #14144, .F. ) ;
#11308 = CARTESIAN_POINT ( 'NONE',  ( 0.000000000000000000, 0.000000000000000000, 2.500000000000000000 ) ) ;
#11309 = EDGE_LOOP ( 'NONE', ( #17782, #1912, #12237, #887 ) ) ;
#11310 = CARTESIAN_POINT ( 'NONE',  ( 39.00000000000000000, 29.49999999999999645, 12.00000000000000000 ) ) ;
#11311 = ADVANCED_BREP_SHAPE_REPRESENTATION ( '', ( #2432, #8005 ), #18550 ) ;
#11312 = PLANE ( 'NONE',  #10224 ) ;
#11313 = LINE ( 'NONE', #6218, #15023 ) ;
#11314 = DIRECTION ( 'NONE',  ( -1.000000000000000000, -1.224606353822377258E-16, -0.000000000000000000 ) ) ;
#11315 = AXIS2_PLACEMENT_3D ( 'NONE', #20094, #16657, #12982 ) ;
#11316 = ADVANCED_FACE ( 'NONE', ( #17596 ), #12092, .T. ) ;
#11317 = CARTESIAN_POINT ( 'NONE',  ( -9.500000000000211386, 3.086737114211961064, -6.959589141758143249 ) ) ;
#11318 = CARTESIAN_POINT ( 'NONE',  ( 29.00000000000000000, -29.50000000000000355, 11.50000000000000000 ) ) ;
#11319 = EDGE_LOOP ( 'NONE', ( #109, #14937 ) ) ;
#11320 = LINE ( 'NONE', #9634, #8293 ) ;
#11321 = CARTESIAN_POINT ( 'NONE',  ( -8.000000000000021316, 1.040949779275251323E-15, 0.000000000000000000 ) ) ;
#11322 = FACE_OUTER_BOUND ( 'NONE', #6179, .T. ) ;
#11323 = DIRECTION ( 'NONE',  ( 0.000000000000000000, 1.000000000000000000, 0.000000000000000000 ) ) ;
#11324 = DIRECTION ( 'NONE',  ( 1.000000000000000000, -0.000000000000000000, -0.000000000000000000 ) ) ;
#11325 = CARTESIAN_POINT ( 'NONE',  ( 29.00000000000000000, 29.50000000000000355, 11.50000000000000000 ) ) ;
#11326 = DIRECTION ( 'NONE',  ( -1.000000000000000000, 0.000000000000000000, 0.000000000000000000 ) ) ;
#11327 = CIRCLE ( 'NONE', #2413, 4.000000000000000000 ) ;
#11328 = ORIENTED_EDGE ( 'NONE', *, *, #6578, .F. ) ;
#11329 = CARTESIAN_POINT ( 'NONE',  ( 0.000000000000000000, 0.000000000000000000, 15.50000000000000000 ) ) ;
#11330 = PLANE ( 'NONE',  #20364 ) ;
#11331 = AXIS2_PLACEMENT_3D ( 'NONE', #7821, #17234, #4080 ) ;
#11332 = CARTESIAN_POINT ( 'NONE',  ( 86.51113724927145654, -4.999999999999989342, 0.000000000000000000 ) ) ;
#11333 = EDGE_CURVE ( 'NONE', #6140, #21092, #11747, .T. ) ;
#11334 = DIRECTION ( 'NONE',  ( -0.5735764363510519326, 0.8191520442889876907, 1.003171929053519816E-16 ) ) ;
#11335 = ORIENTED_EDGE ( 'NONE', *, *, #14788, .T. ) ;
#11336 = EDGE_LOOP ( 'NONE', ( #7062, #6537, #16999, #23831 ) ) ;
#11337 = CONTEXT_DEPENDENT_SHAPE_REPRESENTATION ( #15890, #21729 ) ;
#11338 = EDGE_CURVE ( 'NONE', #8624, #11364, #882, .T. ) ;
#11339 = VERTEX_POINT ( 'NONE', #23244 ) ;
#11340 = DIRECTION ( 'NONE',  ( 1.000000000000000000, 0.000000000000000000, -0.000000000000000000 ) ) ;
#11341 = CARTESIAN_POINT ( 'NONE',  ( 23.00000000000000000, 2.119223430970398336, -17.74893002550478016 ) ) ;
#11342 = EDGE_CURVE ( 'NONE', #1207, #19938, #19703, .T. ) ;
#11343 = CARTESIAN_POINT ( 'NONE',  ( 3.890962118697714531E-15, 15.50000000000000000, -40.80000000000000426 ) ) ;
#11344 = ORIENTED_EDGE ( 'NONE', *, *, #21075, .F. ) ;
#11345 = CIRCLE ( 'NONE', #875, 5.000000000000007994 ) ;
#11346 = EDGE_LOOP ( 'NONE', ( #16564, #14201, #10346, #6269 ) ) ;
#11347 = AXIS2_PLACEMENT_3D ( 'NONE', #14271, #19892, #23685 ) ;
#11348 = AXIS2_PLACEMENT_3D ( 'NONE', #14127, #12296, #14245 ) ;
#11349 = CARTESIAN_POINT ( 'NONE',  ( -28.99999999999999645, -29.50000000000001066, 27.00000000000000000 ) ) ;
#11350 = AXIS2_PLACEMENT_3D ( 'NONE', #14182, #23105, #13959 ) ;
#11351 = EDGE_LOOP ( 'NONE', ( #5297, #16921, #3344, #12191 ) ) ;
#11352 = AXIS2_PLACEMENT_3D ( 'NONE', #16747, #1647, #9199 ) ;
#11353 = VECTOR ( 'NONE', #23701, 1000.000000000000000 ) ;
#11354 = EDGE_LOOP ( 'NONE', ( #13971, #9666, #10984, #23842 ) ) ;
#11355 = CARTESIAN_POINT ( 'NONE',  ( -31.74999999999995737, 0.000000000000000000, 0.000000000000000000 ) ) ;
#11356 = DIRECTION ( 'NONE',  ( -0.000000000000000000, 0.000000000000000000, 1.000000000000000000 ) ) ;
#11357 =( BOUNDED_CURVE ( )  B_SPLINE_CURVE ( 3, ( #20269, #10955, #18432, #19912 ),
 .UNSPECIFIED., .F., .T. ) 
 B_SPLINE_CURVE_WITH_KNOTS ( ( 4, 4 ),
 ( 1.570796326794895670, 3.141592653589793116 ),
 .UNSPECIFIED. ) 
 CURVE ( )  GEOMETRIC_REPRESENTATION_ITEM ( )  RATIONAL_B_SPLINE_CURVE ( ( 1.000000000000000000, 0.8047378541243648264, 0.8047378541243648264, 1.000000000000000000 ) ) 
 REPRESENTATION_ITEM ( '' )  );
#11358 = DIRECTION ( 'NONE',  ( 1.000000000000000000, 0.000000000000000000, 0.000000000000000000 ) ) ;
#11359 = ORIENTED_EDGE ( 'NONE', *, *, #902, .T. ) ;
#11360 = ORIENTED_EDGE ( 'NONE', *, *, #15527, .T. ) ;
#11361 = FACE_OUTER_BOUND ( 'NONE', #698, .T. ) ;
#11362 = CARTESIAN_POINT ( 'NONE',  ( 28.27483331787888332, -41.23752903419610050, 11.00000000000000000 ) ) ;
#11363 = DIRECTION ( 'NONE',  ( -1.000000000000000000, 0.000000000000000000, 0.000000000000000000 ) ) ;
#11364 = VERTEX_POINT ( 'NONE', #12353 ) ;
#11365 = ORIENTED_EDGE ( 'NONE', *, *, #6519, .F. ) ;
#11366 = CARTESIAN_POINT ( 'NONE',  ( -5.365059087798939252, -7.384370330707086261, 3.933165578109188321 ) ) ;
#11367 = EDGE_CURVE ( 'NONE', #7050, #21802, #16446, .T. ) ;
#11368 = ORIENTED_EDGE ( 'NONE', *, *, #19910, .F. ) ;
#11369 = AXIS2_PLACEMENT_3D ( 'NONE', #16417, #1800, #18161 ) ;
#11370 = CONICAL_SURFACE ( 'NONE', #2046, 5.000000000000007994, 0.9599310885968855844 ) ;
#11371 = CIRCLE ( 'NONE', #22707, 20.85000000000000853 ) ;
#11372 = VECTOR ( 'NONE', #22667, 1000.000000000000000 ) ;
#11373 = PRODUCT_CONTEXT ( 'NONE', #3234, 'mechanical' ) ;
#11374 = VECTOR ( 'NONE', #1568, 1000.000000000000000 ) ;
#11375 = EDGE_CURVE ( 'NONE', #17477, #530, #8328, .T. ) ;
#11376 = AXIS2_PLACEMENT_3D ( 'NONE', #1720, #1842, #20509 ) ;
#11377 = EDGE_LOOP ( 'NONE', ( #19917, #12388, #8414, #5260 ) ) ;
#11378 = ORIENTED_EDGE ( 'NONE', *, *, #4905, .T. ) ;
#11379 = EDGE_CURVE ( 'NONE', #3226, #20146, #15245, .T. ) ;
#11380 = CARTESIAN_POINT ( 'NONE',  ( -34.00000000000000000, -3.999999999999999112, 9.500000000000000000 ) ) ;
#11381 = CARTESIAN_POINT ( 'NONE',  ( 6.222797240145152671E-13, -9.127583699786111282, -8.133165578109188942 ) ) ;
#11382 = EDGE_CURVE ( 'NONE', #13748, #21366, #4775, .T. ) ;
#11383 = ADVANCED_FACE ( 'NONE', ( #4940 ), #7844, .T. ) ;
#11384 = CIRCLE ( 'NONE', #20369, 5.000000000000007994 ) ;
#11385 = CARTESIAN_POINT ( 'NONE',  ( 76.32931906745326955, 7.420530141404717394E-15, 0.000000000000000000 ) ) ;
#11386 = ORIENTED_EDGE ( 'NONE', *, *, #23259, .T. ) ;
#11387 = DIRECTION ( 'NONE',  ( -0.000000000000000000, -0.000000000000000000, -1.000000000000000000 ) ) ;
#11388 = DIRECTION ( 'NONE',  ( -0.000000000000000000, -0.000000000000000000, -1.000000000000000000 ) ) ;
#11389 = LINE ( 'NONE', #2637, #9061 ) ;
#11390 = DIRECTION ( 'NONE',  ( -1.000000000000000000, -0.000000000000000000, -0.000000000000000000 ) ) ;
#11391 = DIRECTION ( 'NONE',  ( 0.5735764363510427177, -0.8191520442889941300, 1.003171929053527705E-16 ) ) ;
#11392 = LINE ( 'NONE', #23013, #2064 ) ;
#11393 = AXIS2_PLACEMENT_3D ( 'NONE', #567, #13236, #15440 ) ;
#11394 = CIRCLE ( 'NONE', #7900, 10.94716442891539465 ) ;
#11395 = EDGE_LOOP ( 'NONE', ( #2020, #12151, #18478, #20016 ) ) ;
#11396 = DIRECTION ( 'NONE',  ( 0.000000000000000000, 0.000000000000000000, 1.000000000000000000 ) ) ;
#11397 = CIRCLE ( 'NONE', #511, 8.999999999999998224 ) ;
#11398 = DIRECTION ( 'NONE',  ( 1.000000000000000000, 0.000000000000000000, -0.000000000000000000 ) ) ;
#11399 = CARTESIAN_POINT ( 'NONE',  ( 16.36913330654532217, 6.602951766536810041, -6.845624079409801332 ) ) ;
#11400 = VECTOR ( 'NONE', #23212, 1000.000000000000000 ) ;
#11401 = VECTOR ( 'NONE', #11220, 1000.000000000000000 ) ;
#11402 = FACE_OUTER_BOUND ( 'NONE', #8903, .T. ) ;
#11403 = CYLINDRICAL_SURFACE ( 'NONE', #20782, 14.72592346043842326 ) ;
#11404 = AXIS2_PLACEMENT_3D ( 'NONE', #665, #22552, #5833 ) ;
#11405 = FILL_AREA_STYLE_COLOUR ( '', #14816 ) ;
#11406 = EDGE_LOOP ( 'NONE', ( #17817, #3872 ) ) ;
#11407 = ADVANCED_FACE ( 'NONE', ( #15597 ), #473, .T. ) ;
#11408 = VERTEX_POINT ( 'NONE', #9986 ) ;
#11409 = ORIENTED_EDGE ( 'NONE', *, *, #1614, .T. ) ;
#11410 = ORIENTED_EDGE ( 'NONE', *, *, #8287, .T. ) ;
#11411 = AXIS2_PLACEMENT_3D ( 'NONE', #11298, #14979, #18662 ) ;
#11412 = EDGE_LOOP ( 'NONE', ( #791, #2704, #13599, #10157 ) ) ;
#11413 = FACE_OUTER_BOUND ( 'NONE', #1448, .T. ) ;
#11414 = CARTESIAN_POINT ( 'NONE',  ( -10.00000000000000000, 0.000000000000000000, 0.000000000000000000 ) ) ;
#11415 = ADVANCED_FACE ( 'NONE', ( #13283 ), #11449, .F. ) ;
#11416 = AXIS2_PLACEMENT_3D ( 'NONE', #19578, #4587, #2856 ) ;
#11417 = CIRCLE ( 'NONE', #13784, 18.50000000000000000 ) ;
#11418 = CARTESIAN_POINT ( 'NONE',  ( 5.871322893124551356, -8.081182679343980269, -10.90674201446023339 ) ) ;
#11419 = CARTESIAN_POINT ( 'NONE',  ( 40.23082370883257397, -27.62204025492844650, -3.000000000000000000 ) ) ;
#11420 = SURFACE_STYLE_USAGE ( .BOTH. , #22205 ) ;
#11421 = DIRECTION ( 'NONE',  ( -1.000000000000000000, 0.000000000000000000, 0.000000000000000000 ) ) ;
#11422 = VECTOR ( 'NONE', #6183, 1000.000000000000000 ) ;
#11423 = AXIS2_PLACEMENT_3D ( 'NONE', #14458, #3608, #14938 ) ;
#11424 = DIRECTION ( 'NONE',  ( 0.000000000000000000, 1.000000000000000000, 0.000000000000000000 ) ) ;
#11425 = ORIENTED_EDGE ( 'NONE', *, *, #7082, .T. ) ;
#11426 = CARTESIAN_POINT ( 'NONE',  ( -39.99999999999999289, -27.79189783386527779, -27.00000000000000000 ) ) ;
#11427 = DIRECTION ( 'NONE',  ( 0.000000000000000000, 0.000000000000000000, 1.000000000000000000 ) ) ;
#11428 = CARTESIAN_POINT ( 'NONE',  ( -36.00000000000001421, 50.99999999999999289, 12.50000000000000000 ) ) ;
#11429 = CARTESIAN_POINT ( 'NONE',  ( 4.489900896931573904, 1.377380391735520653E-15, -11.24716442891539359 ) ) ;
#11430 = DIRECTION ( 'NONE',  ( -5.501724186093585079E-16, -1.000000000000000000, 0.000000000000000000 ) ) ;
#11431 = DIRECTION ( 'NONE',  ( 0.000000000000000000, 0.9096319953545193293, -0.4154150130018842701 ) ) ;
#11432 = AXIS2_PLACEMENT_3D ( 'NONE', #3655, #11067, #16704 ) ;
#11433 = ORIENTED_EDGE ( 'NONE', *, *, #17384, .T. ) ;
#11434 = DIRECTION ( 'NONE',  ( 0.000000000000000000, -1.000000000000000000, 0.000000000000000000 ) ) ;
#11435 = AXIS2_PLACEMENT_3D ( 'NONE', #11679, #9728, #13545 ) ;
#11436 = VERTEX_POINT ( 'NONE', #6108 ) ;
#11437 = EDGE_CURVE ( 'NONE', #12531, #15133, #9044, .T. ) ;
#11438 = CARTESIAN_POINT ( 'NONE',  ( 9.499999999999790390, 3.086737114213260025, 10.15958914175814520 ) ) ;
#11439 = VECTOR ( 'NONE', #163, 1000.000000000000000 ) ;
#11440 = AXIS2_PLACEMENT_3D ( 'NONE', #21670, #21893, #20193 ) ;
#11441 = CIRCLE ( 'NONE', #13803, 5.100000000000000533 ) ;
#11442 = EDGE_LOOP ( 'NONE', ( #14482, #8658, #9679, #5179 ) ) ;
#11443 = DIRECTION ( 'NONE',  ( 0.000000000000000000, 0.000000000000000000, 1.000000000000000000 ) ) ;
#11444 = CARTESIAN_POINT ( 'NONE',  ( -41.50000000000000000, -28.80990663662250739, 11.00000000000000000 ) ) ;
#11445 = CIRCLE ( 'NONE', #7945, 9.000000000000000000 ) ;
#11446 = CARTESIAN_POINT ( 'NONE',  ( 7.999999999999992895, 9.797174393178817769E-16, 105.0000000000000000 ) ) ;
#11447 = DIRECTION ( 'NONE',  ( 1.000000000000000000, 4.613626265895764052E-16, -0.000000000000000000 ) ) ;
#11448 = EDGE_CURVE ( 'NONE', #11678, #1599, #14108, .T. ) ;
#11449 = CYLINDRICAL_SURFACE ( 'NONE', #9027, 4.499999999999997335 ) ;
#11450 = AXIS2_PLACEMENT_3D ( 'NONE', #1489, #10947, #20495 ) ;
#11451 = CARTESIAN_POINT ( 'NONE',  ( -5.871322893124554021, 8.081182679343978492, -2.759589141758142627 ) ) ;
#11452 = VERTEX_POINT ( 'NONE', #15221 ) ;
#11453 = AXIS2_PLACEMENT_3D ( 'NONE', #19801, #12688, #20154 ) ;
#11454 = DIRECTION ( 'NONE',  ( 0.000000000000000000, 1.000000000000000000, 0.000000000000000000 ) ) ;
#11455 = VERTEX_POINT ( 'NONE', #19288 ) ;
#11456 = PLANE ( 'NONE',  #18821 ) ;
#11457 = AXIS2_PLACEMENT_3D ( 'NONE', #4611, #19485, #8365 ) ;
#11458 = CARTESIAN_POINT ( 'NONE',  ( 2.844687509167349138, 8.538973046698279390, 80.02720063512431636 ) ) ;
#11459 = SURFACE_STYLE_FILL_AREA ( #4179 ) ;
#11460 = CIRCLE ( 'NONE', #6039, 15.00000000000000000 ) ;
#11461 = DIRECTION ( 'NONE',  ( -1.000000000000000000, -0.000000000000000000, -0.000000000000000000 ) ) ;
#11462 = CARTESIAN_POINT ( 'NONE',  ( 10.00000000000000533, 15.50000000000000000, -40.80000000000000426 ) ) ;
#11463 = EDGE_CURVE ( 'NONE', #569, #886, #17446, .T. ) ;
#11464 = CARTESIAN_POINT ( 'NONE',  ( 0.000000000000000000, 0.000000000000000000, 0.000000000000000000 ) ) ;
#11465 = DIRECTION ( 'NONE',  ( -0.000000000000000000, -0.000000000000000000, -1.000000000000000000 ) ) ;
#11466 = DIRECTION ( 'NONE',  ( -0.000000000000000000, -0.000000000000000000, -1.000000000000000000 ) ) ;
#11467 = VERTEX_POINT ( 'NONE', #9626 ) ;
#11468 = CARTESIAN_POINT ( 'NONE',  ( 60.32931906745326245, 5.000000000000016875, 6.123233995736777129E-16 ) ) ;
#11469 = ADVANCED_FACE ( 'NONE', ( #4170 ), #2572, .T. ) ;
#11470 = CARTESIAN_POINT ( 'NONE',  ( 6.222797240145152671E-13, -9.127583699786111282, 8.133165578109188942 ) ) ;
#11471 = DIRECTION ( 'NONE',  ( 0.000000000000000000, -1.000000000000000000, 0.000000000000000000 ) ) ;
#11472 = ADVANCED_FACE ( 'NONE', ( #4539 ), #17074, .T. ) ;
#11473 = CARTESIAN_POINT ( 'NONE',  ( 20.85000000000000853, 15.03999999999999915, -25.00000000000000000 ) ) ;
#11474 = APPLICATION_CONTEXT ( 'automotive_design' ) ;
#11475 = ORIENTED_EDGE ( 'NONE', *, *, #15034, .T. ) ;
#11476 = ADVANCED_FACE ( 'NONE', ( #4036 ), #743, .F. ) ;
#11477 = EDGE_LOOP ( 'NONE', ( #17461, #15314, #15081, #19164, #5271 ) ) ;
#11478 = CIRCLE ( 'NONE', #8382, 5.000000000000007994 ) ;
#11479 = AXIS2_PLACEMENT_3D ( 'NONE', #23936, #16247, #14291 ) ;
#11480 = ORIENTED_EDGE ( 'NONE', *, *, #3572, .F. ) ;
#11481 = ITEM_DEFINED_TRANSFORMATION ( 'NONE', 'NONE', #2984,  #8005 ) ;
#11482 = VERTEX_POINT ( 'NONE', #495 ) ;
#11483 = DIRECTION ( 'NONE',  ( 0.000000000000000000, 0.000000000000000000, 1.000000000000000000 ) ) ;
#11484 = AXIS2_PLACEMENT_3D ( 'NONE', #17820, #850, #14138 ) ;
#11485 = CONICAL_SURFACE ( 'NONE', #5664, 7.999999999999992895, 0.7853981633974439491 ) ;
#11486 = VECTOR ( 'NONE', #7523, 1000.000000000000000 ) ;
#11487 = CARTESIAN_POINT ( 'NONE',  ( 9.499999999999790390, 3.086737114213260025, 9.306742014460233747 ) ) ;
#11488 = ORIENTED_EDGE ( 'NONE', *, *, #3971, .F. ) ;
#11489 = ORIENTED_EDGE ( 'NONE', *, *, #9905, .F. ) ;
#11490 = DIRECTION ( 'NONE',  ( -0.000000000000000000, -0.000000000000000000, -1.000000000000000000 ) ) ;
#11491 = EDGE_LOOP ( 'NONE', ( #14425, #14582, #17067, #15241 ) ) ;
#11492 = VERTEX_POINT ( 'NONE', #7912 ) ;
#11493 = FACE_OUTER_BOUND ( 'NONE', #9161, .T. ) ;
#11494 = FACE_BOUND ( 'NONE', #11569, .T. ) ;
#11495 = CARTESIAN_POINT ( 'NONE',  ( 4.029965094393306726E-41, -5.916456789157588541E-28, -12.50000000000000000 ) ) ;
#11496 = AXIS2_PLACEMENT_3D ( 'NONE', #2197, #2430, #736 ) ;
#11497 = CIRCLE ( 'NONE', #23615, 5.000000000000007994 ) ;
#11498 = CARTESIAN_POINT ( 'NONE',  ( 24.75000000000000711, 29.50000000000000000, 14.00000000000000178 ) ) ;
#11499 = VERTEX_POINT ( 'NONE', #7785 ) ;
#11500 = CARTESIAN_POINT ( 'NONE',  ( 35.99999999999999289, -51.00000000000000711, 12.50000000000000000 ) ) ;
#11501 = EDGE_CURVE ( 'NONE', #2036, #4703, #625, .T. ) ;
#11502 = DIRECTION ( 'NONE',  ( -0.7089874389501490404, -0.7052211081716915908, 0.000000000000000000 ) ) ;
#11503 = ADVANCED_FACE ( 'NONE', ( #19159 ), #9792, .T. ) ;
#11504 = DIRECTION ( 'NONE',  ( -1.000000000000000000, 0.000000000000000000, -0.000000000000000000 ) ) ;
#11505 = VERTEX_POINT ( 'NONE', #15485 ) ;
#11506 = CIRCLE ( 'NONE', #1024, 13.72592346138681130 ) ;
#11507 = VECTOR ( 'NONE', #11504, 1000.000000000000000 ) ;
#11508 = ORIENTED_EDGE ( 'NONE', *, *, #20243, .F. ) ;
#11509 = CARTESIAN_POINT ( 'NONE',  ( 5.365059087799946447, -7.384370330706356178, 4.333165578109189120 ) ) ;
#11510 = ORIENTED_EDGE ( 'NONE', *, *, #11902, .F. ) ;
#11511 = VERTEX_POINT ( 'NONE', #377 ) ;
#11512 = DIRECTION ( 'NONE',  ( 0.5735764363510427177, -0.8191520442889941300, 1.003171929053527705E-16 ) ) ;
#11513 = ORIENTED_EDGE ( 'NONE', *, *, #5020, .F. ) ;
#11514 = EDGE_LOOP ( 'NONE', ( #15822, #3020, #6265, #17219 ) ) ;
#11515 = DIRECTION ( 'NONE',  ( 1.000000000000000000, 4.625929269271481378E-15, 0.000000000000000000 ) ) ;
#11516 = CARTESIAN_POINT ( 'NONE',  ( -8.680847955711007202, -5.923547351154968927E-13, -9.633165578109188942 ) ) ;
#11517 = AXIS2_PLACEMENT_3D ( 'NONE', #15837, #11782, #6307 ) ;
#11518 = CARTESIAN_POINT ( 'NONE',  ( -31.74999999999995737, 0.000000000000000000, 0.000000000000000000 ) ) ;
#11519 = AXIS2_PLACEMENT_3D ( 'NONE', #9980, #23056, #13788 ) ;
#11520 = ORIENTED_EDGE ( 'NONE', *, *, #20776, .T. ) ;
#11521 = DIRECTION ( 'NONE',  ( 0.7071067811865474617, 8.659560562354932858E-17, -0.7071067811865474617 ) ) ;
#11522 = FACE_OUTER_BOUND ( 'NONE', #20242, .T. ) ;
#11523 = CARTESIAN_POINT ( 'NONE',  ( 41.99999999999999289, 5.618459588085056979E-15, 0.000000000000000000 ) ) ;
#11524 = CARTESIAN_POINT ( 'NONE',  ( 23.00000000000000000, 8.890849273385601492, 7.584660931657517757 ) ) ;
#11525 = LINE ( 'NONE', #6055, #8506 ) ;
#11526 = CIRCLE ( 'NONE', #21695, 20.85000000000000142 ) ;
#11527 = FACE_OUTER_BOUND ( 'NONE', #9083, .T. ) ;
#11528 = EDGE_CURVE ( 'NONE', #15317, #16244, #13551, .T. ) ;
#11529 = ORIENTED_EDGE ( 'NONE', *, *, #4231, .F. ) ;
#11530 = DIRECTION ( 'NONE',  ( 1.000000000000000000, 0.000000000000000000, 0.000000000000000000 ) ) ;
#11531 = SURFACE_SIDE_STYLE ('',( #2645 ) ) ;
#11532 = FACE_OUTER_BOUND ( 'NONE', #7607, .T. ) ;
#11533 = FACE_OUTER_BOUND ( 'NONE', #5689, .T. ) ;
#11534 = EDGE_CURVE ( 'NONE', #14876, #17470, #19967, .T. ) ;
#11535 = CARTESIAN_POINT ( 'NONE',  ( 23.00000000000000000, -9.239931321968246181, 10.79948145182496511 ) ) ;
#11536 = ADVANCED_FACE ( 'NONE', ( #13662 ), #18788, .T. ) ;
#11537 = LINE ( 'NONE', #15313, #4835 ) ;
#11538 = ADVANCED_FACE ( 'NONE', ( #15111 ), #22576, .F. ) ;
#11539 = CIRCLE ( 'NONE', #1053, 5.000000000000007994 ) ;
#11540 = CARTESIAN_POINT ( 'NONE',  ( -5.871322893123449127, -8.081182679344781405, 8.506742014460233037 ) ) ;
#11541 = ORIENTED_EDGE ( 'NONE', *, *, #3298, .F. ) ;
#11542 = CIRCLE ( 'NONE', #9197, 5.000000000000007994 ) ;
#11543 = EDGE_LOOP ( 'NONE', ( #16498, #7356, #3386, #13235, #10854 ) ) ;
#11544 = ORIENTED_EDGE ( 'NONE', *, *, #14597, .T. ) ;
#11545 = DIRECTION ( 'NONE',  ( 2.775557561562889502E-17, -2.428612866367533014E-17, -1.000000000000000000 ) ) ;
#11546 = CIRCLE ( 'NONE', #1063, 8.999999999999998224 ) ;
#11547 = ORIENTED_EDGE ( 'NONE', *, *, #12970, .T. ) ;
#11548 = DIRECTION ( 'NONE',  ( -0.000000000000000000, -0.000000000000000000, -1.000000000000000000 ) ) ;
#11549 = UNCERTAINTY_MEASURE_WITH_UNIT (LENGTH_MEASURE( 1.000000000000000082E-05 ), #5941, 'distance_accuracy_value', 'NONE');
#11550 = AXIS2_PLACEMENT_3D ( 'NONE', #19841, #3110, #5068 ) ;
#11551 = CARTESIAN_POINT ( 'NONE',  ( 3.934052222107095265, -8.094642247421083070, 12.50000000000000000 ) ) ;
#11552 = LINE ( 'NONE', #7211, #22453 ) ;
#11553 = CARTESIAN_POINT ( 'NONE',  ( 43.49999999999997868, -25.84341543330623381, 0.000000000000000000 ) ) ;
#11554 = CARTESIAN_POINT ( 'NONE',  ( 2.935661446561383503, 9.035036904804158553, -5.606742014460233570 ) ) ;
#11555 = EDGE_LOOP ( 'NONE', ( #18291, #2152, #3400, #13350, #13553, #14288 ) ) ;
#11556 = CONICAL_SURFACE ( 'NONE', #13527, 4.172000000000008590, 0.9599310885968742602 ) ;
#11557 = DIRECTION ( 'NONE',  ( -0.000000000000000000, -0.000000000000000000, -1.000000000000000000 ) ) ;
#11558 = EDGE_CURVE ( 'NONE', #1654, #6020, #8640, .T. ) ;
#11559 = ORIENTED_EDGE ( 'NONE', *, *, #8592, .F. ) ;
#11560 = DIRECTION ( 'NONE',  ( 1.000000000000000000, 2.600433232233976523E-16, -0.000000000000000000 ) ) ;
#11561 = CARTESIAN_POINT ( 'NONE',  ( 71.67068093254673045, 7.562528597612068045E-15, 0.000000000000000000 ) ) ;
#11562 = DIRECTION ( 'NONE',  ( -0.000000000000000000, -0.000000000000000000, -1.000000000000000000 ) ) ;
#11563 = CARTESIAN_POINT ( 'NONE',  ( 71.67068093254673045, 5.000000000000015987, 0.000000000000000000 ) ) ;
#11564 = ADVANCED_FACE ( 'NONE', ( #12430 ), #12057, .T. ) ;
#11565 = ORIENTED_EDGE ( 'NONE', *, *, #11294, .F. ) ;
#11566 = EDGE_CURVE ( 'NONE', #6675, #9714, #13325, .T. ) ;
#11567 = LINE ( 'NONE', #7017, #22825 ) ;
#11568 = ORIENTED_EDGE ( 'NONE', *, *, #3892, .F. ) ;
#11569 = EDGE_LOOP ( 'NONE', ( #20677, #9920 ) ) ;
#11570 = CARTESIAN_POINT ( 'NONE',  ( 7.685661446562381371, -5.583959896777971110, 7.859589141758143604 ) ) ;
#11571 = ORIENTED_EDGE ( 'NONE', *, *, #19990, .T. ) ;
#11572 = CARTESIAN_POINT ( 'NONE',  ( 58.57977184163763695, 7.562528597612068045E-15, 0.000000000000000000 ) ) ;
#11573 = CARTESIAN_POINT ( 'NONE',  ( 62.94340820527399671, 7.562528597612068045E-15, 0.000000000000000000 ) ) ;
#11574 = DIRECTION ( 'NONE',  ( -0.000000000000000000, -0.000000000000000000, -1.000000000000000000 ) ) ;
#11575 = CARTESIAN_POINT ( 'NONE',  ( 81.85249911436491743, 7.562528597612068045E-15, 0.000000000000000000 ) ) ;
#11576 = CARTESIAN_POINT ( 'NONE',  ( 6.976272796952845745, -5.349986750954834669, -12.49999999999999467 ) ) ;
#11577 = DIRECTION ( 'NONE',  ( -0.000000000000000000, -1.000000000000000000, -0.000000000000000000 ) ) ;
#11578 = EDGE_LOOP ( 'NONE', ( #15767, #20293, #7432, #6627, #6111, #4751 ) ) ;
#11579 = CARTESIAN_POINT ( 'NONE',  ( 40.00000000000000000, -27.79189783386526358, 27.00000000000000000 ) ) ;
#11580 = ORIENTED_EDGE ( 'NONE', *, *, #20610, .T. ) ;
#11581 = CARTESIAN_POINT ( 'NONE',  ( -7.783282916316068167, -5.092938787329413408, 12.23045887587376690 ) ) ;
#11582 = AXIS2_PLACEMENT_3D ( 'NONE', #5564, #10804, #8750 ) ;
#11583 = CARTESIAN_POINT ( 'NONE',  ( 29.00000000000000000, 29.50000000000000355, 0.000000000000000000 ) ) ;
#11584 = SURFACE_STYLE_USAGE ( .BOTH. , #17333 ) ;
#11585 = VECTOR ( 'NONE', #21641, 1000.000000000000000 ) ;
#11586 = DIRECTION ( 'NONE',  ( -0.5735764363510517105, -0.8191520442889879128, 0.000000000000000000 ) ) ;
#11587 = DIRECTION ( 'NONE',  ( -1.000000000000000000, -1.224606353822377258E-16, -0.000000000000000000 ) ) ;
#11588 = EDGE_CURVE ( 'NONE', #2444, #19429, #23562, .T. ) ;
#11589 = CARTESIAN_POINT ( 'NONE',  ( -31.10231664966676846, 45.36128193761570770, 0.000000000000000000 ) ) ;
#11590 = DIRECTION ( 'NONE',  ( -1.000000000000000000, 0.000000000000000000, 0.000000000000000000 ) ) ;
#11591 = CARTESIAN_POINT ( 'NONE',  ( 7.685661446562381371, -5.583959896777971110, -5.006742014460233037 ) ) ;
#11592 = EDGE_LOOP ( 'NONE', ( #11970, #3519, #3766, #23006 ) ) ;
#11593 = CARTESIAN_POINT ( 'NONE',  ( -34.00000000000000000, -3.851859888774471706E-31, 11.00000000000000000 ) ) ;
#11594 = CARTESIAN_POINT ( 'NONE',  ( -7.022953521754877748, -5.102474405760673015, 7.833165578109188232 ) ) ;
#11595 = DIRECTION ( 'NONE',  ( -0.8757121056631642642, 0.4828336235133042220, 0.000000000000000000 ) ) ;
#11596 = DIRECTION ( 'NONE',  ( -1.000000000000000000, 0.000000000000000000, 0.000000000000000000 ) ) ;
#11597 = AXIS2_PLACEMENT_3D ( 'NONE', #20581, #22536, #17140 ) ;
#11598 = CIRCLE ( 'NONE', #14346, 5.000000000000007994 ) ;
#11599 = CONTEXT_DEPENDENT_SHAPE_REPRESENTATION ( #13055, #18014 ) ;
#11600 = ORIENTED_EDGE ( 'NONE', *, *, #11375, .F. ) ;
#11601 = DIRECTION ( 'NONE',  ( -1.000000000000000000, 0.000000000000000000, 0.000000000000000000 ) ) ;
#11602 = EDGE_CURVE ( 'NONE', #18617, #7700, #21610, .T. ) ;
#11603 = CARTESIAN_POINT ( 'NONE',  ( -6.822232771736903637E-13, 9.988891130263535700, -11.70674201446023410 ) ) ;
#11604 = VERTEX_POINT ( 'NONE', #2805 ) ;
#11605 = ORIENTED_EDGE ( 'NONE', *, *, #11871, .F. ) ;
#11606 = CARTESIAN_POINT ( 'NONE',  ( -19.84999999999999787, 16.67999999999985405, 13.50000000000000178 ) ) ;
#11607 = EDGE_CURVE ( 'NONE', #18707, #18515, #3163, .T. ) ;
#11608 = AXIS2_PLACEMENT_3D ( 'NONE', #23026, #2535, #8375 ) ;
#11609 = LINE ( 'NONE', #11126, #13167 ) ;
#11610 = EDGE_LOOP ( 'NONE', ( #10139, #11992 ) ) ;
#11611 = CARTESIAN_POINT ( 'NONE',  ( -28.99999999999999645, -29.50000000000001066, 27.00000000000000000 ) ) ;
#11612 = EDGE_CURVE ( 'NONE', #8084, #19174, #10364, .T. ) ;
#11613 = ORIENTED_EDGE ( 'NONE', *, *, #19724, .T. ) ;
#11614 = DIRECTION ( 'NONE',  ( 1.000000000000000000, 0.000000000000000000, 0.000000000000000000 ) ) ;
#11615 = FACE_BOUND ( 'NONE', #1873, .T. ) ;
#11616 = CARTESIAN_POINT ( 'NONE',  ( 29.00000000000000000, 29.50000000000000355, 11.50000000000000000 ) ) ;
#11617 = DIRECTION ( 'NONE',  ( -0.000000000000000000, -0.000000000000000000, -1.000000000000000000 ) ) ;
#11618 = EDGE_LOOP ( 'NONE', ( #16516, #20680, #23343 ) ) ;
#11619 = CYLINDRICAL_SURFACE ( 'NONE', #21189, 15.00000000000000000 ) ;
#11620 = DIRECTION ( 'NONE',  ( 1.360567432138674300E-16, -1.000000000000000000, 0.000000000000000000 ) ) ;
#11621 = VERTEX_POINT ( 'NONE', #8281 ) ;
#11622 = ORIENTED_EDGE ( 'NONE', *, *, #9298, .F. ) ;
#11623 = CARTESIAN_POINT ( 'NONE',  ( -9.500000000000000000, -6.482511860946779655E-13, 11.05958914175814556 ) ) ;
#11624 = ORIENTED_EDGE ( 'NONE', *, *, #23788, .T. ) ;
#11625 = CIRCLE ( 'NONE', #14759, 17.87500000001787726 ) ;
#11626 = CARTESIAN_POINT ( 'NONE',  ( 7.685661446562381371, -5.583959896777971110, 5.859589141758143604 ) ) ;
#11627 = ORIENTED_EDGE ( 'NONE', *, *, #10442, .T. ) ;
#11628 = ORIENTED_EDGE ( 'NONE', *, *, #20051, .T. ) ;
#11629 = LINE ( 'NONE', #19100, #20769 ) ;
#11630 = CARTESIAN_POINT ( 'NONE',  ( 8.680847955711007202, 5.912916378492122225E-13, -4.633165578109188942 ) ) ;
#11631 = EDGE_CURVE ( 'NONE', #6073, #5560, #3062, .T. ) ;
#11632 = EDGE_LOOP ( 'NONE', ( #19802, #8905, #2916, #23318, #22113 ) ) ;
#11633 = CARTESIAN_POINT ( 'NONE',  ( -23.97499999999999787, -29.50000000000000000, -3.000000000000000000 ) ) ;
#11634 = CARTESIAN_POINT ( 'NONE',  ( 0.000000000000000000, 0.000000000000000000, 0.000000000000000000 ) ) ;
#11635 = CARTESIAN_POINT ( 'NONE',  ( 81.27272727272728048, 7.491529369508391930E-15, 0.000000000000000000 ) ) ;
#11636 = EDGE_CURVE ( 'NONE', #8495, #23675, #3220, .T. ) ;
#11637 = EDGE_CURVE ( 'NONE', #12712, #1878, #2841, .T. ) ;
#11638 = FACE_OUTER_BOUND ( 'NONE', #23127, .T. ) ;
#11639 = CARTESIAN_POINT ( 'NONE',  ( -28.99999999999999645, 29.50000000000000000, 14.00000000000000178 ) ) ;
#11640 = DIRECTION ( 'NONE',  ( -1.000000000000000000, 0.000000000000000000, 0.000000000000000000 ) ) ;
#11641 = CARTESIAN_POINT ( 'NONE',  ( 65.85249911436491743, 7.562528597612068045E-15, 0.000000000000000000 ) ) ;
#11642 = VERTEX_POINT ( 'NONE', #12538 ) ;
#11643 = CARTESIAN_POINT ( 'NONE',  ( 81.85249911436491743, 7.562528597612068045E-15, 0.000000000000000000 ) ) ;
#11644 = CARTESIAN_POINT ( 'NONE',  ( -6.153822176767817416E-13, 9.500000000000000000, 2.559589141758142894 ) ) ;
#11645 = CARTESIAN_POINT ( 'NONE',  ( 42.00000000000000000, 0.000000000000000000, 11.00000000000000000 ) ) ;
#11646 = CYLINDRICAL_SURFACE ( 'NONE', #6807, 5.099999999999996980 ) ;
#11647 = AXIS2_PLACEMENT_3D ( 'NONE', #21677, #21792, #16522 ) ;
#11648 = CARTESIAN_POINT ( 'NONE',  ( -40.00000000000000000, 0.000000000000000000, 11.00000000000000000 ) ) ;
#11649 = CARTESIAN_POINT ( 'NONE',  ( 8.680847955711199049, -2.820578480813074496, -10.53316557810918752 ) ) ;
#11650 = PRESENTATION_STYLE_ASSIGNMENT (( #15075 ) ) ;
#11651 = ORIENTED_EDGE ( 'NONE', *, *, #18584, .F. ) ;
#11652 = CARTESIAN_POINT ( 'NONE',  ( 7.022953521755574080, -5.102474405759714671, 10.43316557810918788 ) ) ;
#11653 = ORIENTED_EDGE ( 'NONE', *, *, #16694, .F. ) ;
#11654 = CARTESIAN_POINT ( 'NONE',  ( -1.999999999999996669, -45.00000000000000000, -3.000000000000000000 ) ) ;
#11655 = FACE_OUTER_BOUND ( 'NONE', #19879, .T. ) ;
#11656 = CARTESIAN_POINT ( 'NONE',  ( 0.000000000000000000, 15.03999999999999915, -25.00000000000000000 ) ) ;
#11657 = AXIS2_PLACEMENT_3D ( 'NONE', #9012, #9, #1591 ) ;
#11658 = CARTESIAN_POINT ( 'NONE',  ( 4.379988124296517071, -7.836644668421621773, 12.50000000000000178 ) ) ;
#11659 = CARTESIAN_POINT ( 'NONE',  ( -1.999999999999994449, -45.00000000000000000, -26.97499999999999432 ) ) ;
#11660 = DIRECTION ( 'NONE',  ( -1.000000000000000000, 0.000000000000000000, 0.000000000000000000 ) ) ;
#11661 = EDGE_CURVE ( 'NONE', #10567, #12610, #14381, .T. ) ;
#11662 = EDGE_CURVE ( 'NONE', #6532, #18820, #10233, .T. ) ;
#11663 = VERTEX_POINT ( 'NONE', #8781 ) ;
#11664 = CARTESIAN_POINT ( 'NONE',  ( -40.77574956473004164, 27.49633847812775755, 12.00000000000000000 ) ) ;
#11665 = DIRECTION ( 'NONE',  ( -1.000000000000000000, 0.000000000000000000, 0.000000000000000000 ) ) ;
#11666 = CYLINDRICAL_SURFACE ( 'NONE', #8364, 50.00000000000000000 ) ;
#11667 = EDGE_LOOP ( 'NONE', ( #10448, #9238, #3194, #17909 ) ) ;
#11668 = DIRECTION ( 'NONE',  ( 1.000000000000000000, 0.000000000000000000, 0.000000000000000000 ) ) ;
#11669 = DIRECTION ( 'NONE',  ( -1.000000000000000000, 0.000000000000000000, 0.000000000000000000 ) ) ;
#11670 = DIRECTION ( 'NONE',  ( -0.000000000000000000, -0.000000000000000000, -1.000000000000000000 ) ) ;
#11671 = FACE_OUTER_BOUND ( 'NONE', #20631, .T. ) ;
#11672 = ORIENTED_EDGE ( 'NONE', *, *, #13482, .F. ) ;
#11673 = ORIENTED_EDGE ( 'NONE', *, *, #2852, .T. ) ;
#11674 = ORIENTED_EDGE ( 'NONE', *, *, #6470, .T. ) ;
#11675 = CIRCLE ( 'NONE', #2358, 4.249999999999993783 ) ;
#11676 = CARTESIAN_POINT ( 'NONE',  ( -2.935661446561384391, -9.035036904804158553, 9.459589141758144137 ) ) ;
#11677 = DIRECTION ( 'NONE',  ( -1.000000000000000000, -0.000000000000000000, -0.000000000000000000 ) ) ;
#11678 = VERTEX_POINT ( 'NONE', #5116 ) ;
#11679 = CARTESIAN_POINT ( 'NONE',  ( -41.73082370883257397, -27.62204025492846071, -1.500000000000000000 ) ) ;
#11680 = EDGE_CURVE ( 'NONE', #13276, #4711, #4403, .T. ) ;
#11681 = DIRECTION ( 'NONE',  ( -0.5735764363510517105, -0.8191520442889879128, 0.000000000000000000 ) ) ;
#11682 = DIRECTION ( 'NONE',  ( 0.000000000000000000, -0.000000000000000000, 1.000000000000000000 ) ) ;
#11683 = ORIENTED_EDGE ( 'NONE', *, *, #17052, .T. ) ;
#11684 = CARTESIAN_POINT ( 'NONE',  ( 7.685661446561619314, 5.583959896779020049, 6.259589141758143960 ) ) ;
#11685 = DIRECTION ( 'NONE',  ( 0.000000000000000000, -0.000000000000000000, -1.000000000000000000 ) ) ;
#11686 = CARTESIAN_POINT ( 'NONE',  ( 0.000000000000000000, 0.000000000000000000, 9.725923461386811297 ) ) ;
#11687 = ADVANCED_FACE ( 'NONE', ( #17941 ), #1282, .T. ) ;
#11688 = EDGE_CURVE ( 'NONE', #8545, #18646, #1228, .T. ) ;
#11689 = DIRECTION ( 'NONE',  ( 1.000000000000000000, 0.000000000000000000, 0.000000000000000000 ) ) ;
#11690 = ORIENTED_EDGE ( 'NONE', *, *, #14514, .F. ) ;
#11691 = AXIS2_PLACEMENT_3D ( 'NONE', #23512, #19853, #16047 ) ;
#11692 = DIRECTION ( 'NONE',  ( -9.637352644315594010E-17, -0.000000000000000000, -1.000000000000000000 ) ) ;
#11693 = ORIENTED_EDGE ( 'NONE', *, *, #13137, .F. ) ;
#11694 = FACE_OUTER_BOUND ( 'NONE', #23441, .T. ) ;
#11695 = CARTESIAN_POINT ( 'NONE',  ( -8.478934877242544133, 4.214451526824021244, 12.03486692402043978 ) ) ;
#11696 = CARTESIAN_POINT ( 'NONE',  ( 23.00000000000000000, 0.000000000000000000, 0.000000000000000000 ) ) ;
#11697 = PLANE ( 'NONE',  #16348 ) ;
#11698 = CARTESIAN_POINT ( 'NONE',  ( -1.508256302856378905, 8.874244307610334559, 78.39942206751072717 ) ) ;
#11699 = LINE ( 'NONE', #8165, #7119 ) ;
#11700 = CARTESIAN_POINT ( 'NONE',  ( -5.871322893124554021, 8.081182679343978492, 8.759589141758144848 ) ) ;
#11701 = CARTESIAN_POINT ( 'NONE',  ( -9.500000000000211386, 3.086737114211961064, -4.106742014460232681 ) ) ;
#11702 = ORIENTED_EDGE ( 'NONE', *, *, #3862, .T. ) ;
#11703 = DIRECTION ( 'NONE',  ( -0.000000000000000000, -0.000000000000000000, -1.000000000000000000 ) ) ;
#11704 = CARTESIAN_POINT ( 'NONE',  ( 8.680847955710813579, 2.820578480814259326, 10.73316557810918681 ) ) ;
#11705 = CARTESIAN_POINT ( 'NONE',  ( 0.000000000000000000, 0.000000000000000000, 0.000000000000000000 ) ) ;
#11706 = CARTESIAN_POINT ( 'NONE',  ( 0.000000000000000000, -45.00000000000000000, -8.673617379884035472E-16 ) ) ;
#11707 = EDGE_CURVE ( 'NONE', #17720, #23803, #21480, .T. ) ;
#11708 = DIRECTION ( 'NONE',  ( -0.000000000000000000, -0.000000000000000000, -1.000000000000000000 ) ) ;
#11709 = VECTOR ( 'NONE', #14498, 1000.000000000000114 ) ;
#11710 = AXIS2_PLACEMENT_3D ( 'NONE', #24007, #18745, #20116 ) ;
#11711 = ORIENTED_EDGE ( 'NONE', *, *, #7942, .T. ) ;
#11712 = EDGE_LOOP ( 'NONE', ( #10384, #9241, #21667, #2751 ) ) ;
#11713 = CARTESIAN_POINT ( 'NONE',  ( 28.99999999999999645, 29.49999999999999645, -1.500000000000000000 ) ) ;
#11714 = ADVANCED_FACE ( 'NONE', ( #21728 ), #12187, .F. ) ;
#11715 = CARTESIAN_POINT ( 'NONE',  ( 2.935661446562616295, -9.035036904803758873, -8.806742014460233747 ) ) ;
#11716 = ORIENTED_EDGE ( 'NONE', *, *, #10473, .T. ) ;
#11717 = CARTESIAN_POINT ( 'NONE',  ( -40.50000000000000711, 50.99999999999999289, 0.5000000000000004441 ) ) ;
#11718 = CARTESIAN_POINT ( 'NONE',  ( 42.00000000000000000, -6.000000000000015099, 11.00000000000000000 ) ) ;
#11719 = DIRECTION ( 'NONE',  ( -0.8571673007021116675, 0.000000000000000000, -0.5150380749100552658 ) ) ;
#11720 = VERTEX_POINT ( 'NONE', #7303 ) ;
#11721 = CARTESIAN_POINT ( 'NONE',  ( -9.499999999999962697, -8.297908579805900909E-07, -3.500254135480583617 ) ) ;
#11722 = AXIS2_PLACEMENT_3D ( 'NONE', #5609, #13531, #8020 ) ;
#11723 = VERTEX_POINT ( 'NONE', #20139 ) ;
#11724 = CARTESIAN_POINT ( 'NONE',  ( 23.00000000000000000, 0.000000000000000000, 0.000000000000000000 ) ) ;
#11725 = CARTESIAN_POINT ( 'NONE',  ( -35.99999999999995026, 59.99999999999998579, 12.50000000000000000 ) ) ;
#11726 = CIRCLE ( 'NONE', #23062, 5.000000000000007994 ) ;
#11727 = CARTESIAN_POINT ( 'NONE',  ( -10.00000000000000000, 0.000000000000000000, 0.000000000000000000 ) ) ;
#11728 = CARTESIAN_POINT ( 'NONE',  ( -41.73082370883260239, 27.62204025492845361, -1.500000000000000000 ) ) ;
#11729 = ORIENTED_EDGE ( 'NONE', *, *, #23216, .T. ) ;
#11730 = DIRECTION ( 'NONE',  ( -1.000000000000000000, 0.000000000000000000, 0.000000000000000000 ) ) ;
#11731 = DIRECTION ( 'NONE',  ( -0.000000000000000000, -0.000000000000000000, -1.000000000000000000 ) ) ;
#11732 = ORIENTED_EDGE ( 'NONE', *, *, #11286, .F. ) ;
#11733 = ORIENTED_EDGE ( 'NONE', *, *, #10968, .F. ) ;
#11734 = CARTESIAN_POINT ( 'NONE',  ( -2.935661446561384391, -9.035036904804158553, 5.459589141758144137 ) ) ;
#11735 = ORIENTED_EDGE ( 'NONE', *, *, #12965, .T. ) ;
#11736 = EDGE_CURVE ( 'NONE', #15766, #5717, #4795, .T. ) ;
#11737 = VERTEX_POINT ( 'NONE', #11179 ) ;
#11738 =( GEOMETRIC_REPRESENTATION_CONTEXT ( 3 ) GLOBAL_UNCERTAINTY_ASSIGNED_CONTEXT ( ( #1087 ) ) GLOBAL_UNIT_ASSIGNED_CONTEXT ( ( #10598, #7309, #8784 ) ) REPRESENTATION_CONTEXT ( 'NONE', 'WORKASPACE' ) );
#11739 = ORIENTED_EDGE ( 'NONE', *, *, #22981, .T. ) ;
#11740 = ORIENTED_EDGE ( 'NONE', *, *, #1188, .F. ) ;
#11741 = CIRCLE ( 'NONE', #877, 7.999999999999986677 ) ;
#11742 = ADVANCED_FACE ( 'NONE', ( #1482 ), #12160, .T. ) ;
#11743 = AXIS2_PLACEMENT_3D ( 'NONE', #23564, #12321, #19668 ) ;
#11744 = CARTESIAN_POINT ( 'NONE',  ( 76.32931906745326955, 6.123233995736675563E-16, -5.000000000000007994 ) ) ;
#11745 = CARTESIAN_POINT ( 'NONE',  ( 8.680847955710813579, 2.820578480814259326, -6.733165578109187699 ) ) ;
#11746 = EDGE_CURVE ( 'NONE', #702, #23079, #9813, .T. ) ;
#11747 = CIRCLE ( 'NONE', #2418, 12.73082370883260594 ) ;
#11748 = AXIS2_PLACEMENT_3D ( 'NONE', #22159, #14800, #11006 ) ;
#11749 = CARTESIAN_POINT ( 'NONE',  ( 30.32370777929697780, -42.16181938034193877, -1.500000000000000000 ) ) ;
#11750 = ORIENTED_EDGE ( 'NONE', *, *, #21250, .F. ) ;
#11751 = DIRECTION ( 'NONE',  ( -0.000000000000000000, -0.000000000000000000, -1.000000000000000000 ) ) ;
#11752 = DIRECTION ( 'NONE',  ( 0.000000000000000000, 1.000000000000000000, 0.000000000000000000 ) ) ;
#11753 = CARTESIAN_POINT ( 'NONE',  ( 86.21613547800127719, 7.562528597612068045E-15, 0.000000000000000000 ) ) ;
#11754 = DIRECTION ( 'NONE',  ( -1.000000000000000000, 0.000000000000000000, 0.000000000000000000 ) ) ;
#11755 = CYLINDRICAL_SURFACE ( 'NONE', #21422, 1.500000000000000000 ) ;
#11756 = EDGE_LOOP ( 'NONE', ( #5502, #169, #860, #18822 ) ) ;
#11757 = CARTESIAN_POINT ( 'NONE',  ( -41.73082370883257397, -29.50000000000000711, -1.500000000000000000 ) ) ;
#11758 = CARTESIAN_POINT ( 'NONE',  ( -7.685661446561619314, -5.583959896779019161, -6.406742014460233392 ) ) ;
#11759 = ORIENTED_EDGE ( 'NONE', *, *, #14404, .T. ) ;
#11760 = DIRECTION ( 'NONE',  ( -0.000000000000000000, -0.000000000000000000, 1.000000000000000000 ) ) ;
#11761 = PRESENTATION_STYLE_ASSIGNMENT (( #812 ) ) ;
#11762 = CARTESIAN_POINT ( 'NONE',  ( 23.00000000000000000, -6.393861490227802591, -9.782270569456514409 ) ) ;
#11763 = PLANE ( 'NONE',  #23930 ) ;
#11764 = CARTESIAN_POINT ( 'NONE',  ( -7.022953521754877748, -5.102474405760673015, -5.833165578109188232 ) ) ;
#11765 = CIRCLE ( 'NONE', #16833, 8.500000000000000000 ) ;
#11766 = VECTOR ( 'NONE', #17923, 1000.000000000000000 ) ;
#11767 = EDGE_CURVE ( 'NONE', #15771, #3651, #10610, .T. ) ;
#11768 = VECTOR ( 'NONE', #19022, 1000.000000000000000 ) ;
#11769 = CIRCLE ( 'NONE', #20762, 5.100000000000000533 ) ;
#11770 =( LENGTH_UNIT ( ) NAMED_UNIT ( * ) SI_UNIT ( .MILLI., .METRE. ) );
#11771 = ORIENTED_EDGE ( 'NONE', *, *, #23929, .F. ) ;
#11772 = ORIENTED_EDGE ( 'NONE', *, *, #4675, .T. ) ;
#11773 = VECTOR ( 'NONE', #15910, 1000.000000000000114 ) ;
#11774 = EDGE_CURVE ( 'NONE', #23775, #4646, #9062, .T. ) ;
#11775 = CARTESIAN_POINT ( 'NONE',  ( -5.365059087799947335, 7.384370330706355290, 11.33316557810918468 ) ) ;
#11776 = CIRCLE ( 'NONE', #4012, 5.100000000000000533 ) ;
#11777 = ORIENTED_EDGE ( 'NONE', *, *, #12876, .F. ) ;
#11778 = DIRECTION ( 'NONE',  ( 1.000000000000000000, 0.000000000000000000, 0.000000000000000000 ) ) ;
#11779 = VERTEX_POINT ( 'NONE', #14627 ) ;
#11780 = FACE_OUTER_BOUND ( 'NONE', #19041, .T. ) ;
#11781 = CARTESIAN_POINT ( 'NONE',  ( 0.000000000000000000, 11.37860023611340665, 13.78561139983856521 ) ) ;
#11783 = AXIS2_PLACEMENT_3D ( 'NONE', #18243, #12488, #14564 ) ;
#11782 = DIRECTION ( 'NONE',  ( -0.000000000000000000, -0.000000000000000000, 1.000000000000000000 ) ) ;
#11784 = DIRECTION ( 'NONE',  ( 0.000000000000000000, 0.000000000000000000, -1.000000000000000000 ) ) ;
#11785 = AXIS2_PLACEMENT_3D ( 'NONE', #8424, #19536, #17699 ) ;
#11786 = AXIS2_PLACEMENT_3D ( 'NONE', #16515, #16381, #10772 ) ;
#11787 = CIRCLE ( 'NONE', #23125, 9.500000000000000000 ) ;
#11788 = LINE ( 'NONE', #352, #14867 ) ;
#11789 = AXIS2_PLACEMENT_3D ( 'NONE', #17958, #7074, #23454 ) ;
#11790 = PRODUCT_DEFINITION_SHAPE ( 'NONE', 'NONE',  #24123 ) ;
#11791 = DIRECTION ( 'NONE',  ( -1.000000000000000000, -0.000000000000000000, -0.000000000000000000 ) ) ;
#11792 = LINE ( 'NONE', #7035, #7094 ) ;
#11793 = DIRECTION ( 'NONE',  ( 0.000000000000000000, 1.000000000000000000, 0.000000000000000000 ) ) ;
#11794 = AXIS2_PLACEMENT_3D ( 'NONE', #8999, #9346, #16795 ) ;
#11795 = DIRECTION ( 'NONE',  ( 1.000000000000000000, 0.000000000000000000, 0.000000000000000000 ) ) ;
#11796 =( REPRESENTATION_RELATIONSHIP ('NONE','NONE', #21748, #9527 ) REPRESENTATION_RELATIONSHIP_WITH_TRANSFORMATION ( #22726 )SHAPE_REPRESENTATION_RELATIONSHIP( ) );
#11797 = DIRECTION ( 'NONE',  ( 0.000000000000000000, 0.000000000000000000, 1.000000000000000000 ) ) ;
#11798 = ORIENTED_EDGE ( 'NONE', *, *, #21290, .T. ) ;
#11799 = CARTESIAN_POINT ( 'NONE',  ( 8.680847955711199049, -2.820578480813074496, -4.533165578109188409 ) ) ;
#11800 = ORIENTED_EDGE ( 'NONE', *, *, #20597, .F. ) ;
#11801 =( GEOMETRIC_REPRESENTATION_CONTEXT ( 3 ) GLOBAL_UNCERTAINTY_ASSIGNED_CONTEXT ( ( #2775 ) ) GLOBAL_UNIT_ASSIGNED_CONTEXT ( ( #14153, #12907, #5482 ) ) REPRESENTATION_CONTEXT ( 'NONE', 'WORKASPACE' ) );
#11802 = DIRECTION ( 'NONE',  ( 1.000000000000000000, 1.224606353822377258E-16, 0.000000000000000000 ) ) ;
#11803 = EDGE_CURVE ( 'NONE', #13831, #21442, #3415, .T. ) ;
#11804 = DIRECTION ( 'NONE',  ( -1.000000000000000000, 0.000000000000000000, 0.000000000000000000 ) ) ;
#11805 = EDGE_CURVE ( 'NONE', #18394, #5778, #23493, .T. ) ;
#11806 = CIRCLE ( 'NONE', #525, 6.500000000000000888 ) ;
#11807 = ORIENTED_EDGE ( 'NONE', *, *, #13782, .F. ) ;
#11808 = CIRCLE ( 'NONE', #6381, 5.000000000000007994 ) ;
#11809 = DIRECTION ( 'NONE',  ( -0.9160001545545232160, 0.4011779117250717785, -0.000000000000000000 ) ) ;
#11810 = AXIS2_PLACEMENT_3D ( 'NONE', #11385, #4103, #13490 ) ;
#11811 = CIRCLE ( 'NONE', #10646, 50.00000000000000000 ) ;
#11812 = CARTESIAN_POINT ( 'NONE',  ( -14.99999999999999645, 15.50000000000000178, 7.700000000000001954 ) ) ;
#11813 = AXIS2_PLACEMENT_3D ( 'NONE', #2125, #7364, #20564 ) ;
#11814 = DIRECTION ( 'NONE',  ( 9.637352644315592778E-17, 0.000000000000000000, 1.000000000000000000 ) ) ;
#11815 = DIRECTION ( 'NONE',  ( 0.000000000000000000, 0.000000000000000000, 1.000000000000000000 ) ) ;
#11816 = CARTESIAN_POINT ( 'NONE',  ( -40.77574956473004164, 27.49633847812775755, 0.000000000000000000 ) ) ;
#11817 = DIRECTION ( 'NONE',  ( 0.000000000000000000, 1.000000000000000000, 0.000000000000000000 ) ) ;
#11818 = DIRECTION ( 'NONE',  ( 0.000000000000000000, 0.000000000000000000, -1.000000000000000000 ) ) ;
#11819 = ORIENTED_EDGE ( 'NONE', *, *, #3786, .T. ) ;
#11820 = ORIENTED_EDGE ( 'NONE', *, *, #19568, .F. ) ;
#11821 = CARTESIAN_POINT ( 'NONE',  ( 0.000000000000000000, 15.03999999999999915, 25.00000000000000000 ) ) ;
#11822 = CARTESIAN_POINT ( 'NONE',  ( -9.253409020823845310, -1.536709113333740273, 12.15192428665581303 ) ) ;
#11823 = PRODUCT_RELATED_PRODUCT_CATEGORY ( 'part', '', ( #1973 ) ) ;
#11824 = AXIS2_PLACEMENT_3D ( 'NONE', #15011, #13437, #22490 ) ;
#11825 = B_SPLINE_CURVE_WITH_KNOTS ( 'NONE', 3,
 ( #5483, #16233, #18304, #7066, #3067, #16107, #16340, #23568, #10837, #14277, #21966, #3300, #10725, #3171, #23690, #18197, #1488, #21737, #6964, #5253, #1589, #23795 ),
 .UNSPECIFIED., .F., .F.,
 ( 4, 2, 2, 2, 2, 2, 2, 2, 2, 2, 4 ),
 ( 0.4688579448613529044, 0.5352507017536837219, 0.6016434586460146505, 0.6680362155383455791, 0.7012325939845110989, 0.7344289724306765077, 0.8008217293230073253, 0.8672144862153383649, 0.9004108646615036626, 0.9336072431076691824, 1.000000000000000000 ),
 .UNSPECIFIED. ) ;
#11826 = CARTESIAN_POINT ( 'NONE',  ( 64.39795365981944997, 5.000000000000015987, 0.000000000000000000 ) ) ;
#11827 = CARTESIAN_POINT ( 'NONE',  ( 14.67187117805616303, 3.178673068337433349, -8.975236025575915377 ) ) ;
#11828 = EDGE_CURVE ( 'NONE', #12486, #9768, #23786, .T. ) ;
#11829 = VECTOR ( 'NONE', #11838, 1000.000000000000000 ) ;
#11830 = FACE_OUTER_BOUND ( 'NONE', #22926, .T. ) ;
#11831 = CONICAL_SURFACE ( 'NONE', #1351, 4.172000000000008590, 0.9599310885968742602 ) ;
#11832 = CARTESIAN_POINT ( 'NONE',  ( -31.74999999999995737, 0.000000000000000000, 0.000000000000000000 ) ) ;
#11833 = AXIS2_PLACEMENT_3D ( 'NONE', #15432, #19104, #17260 ) ;
#11834 = LINE ( 'NONE', #9745, #18807 ) ;
#11835 = DIRECTION ( 'NONE',  ( 0.5735764363510427177, -0.8191520442889941300, 1.003171929053527705E-16 ) ) ;
#11836 = EDGE_CURVE ( 'NONE', #2505, #5790, #10831, .T. ) ;
#11837 = ORIENTED_EDGE ( 'NONE', *, *, #16614, .F. ) ;
#11838 = DIRECTION ( 'NONE',  ( 0.000000000000000000, 1.000000000000000000, 0.000000000000000000 ) ) ;
#11839 = VECTOR ( 'NONE', #23667, 1000.000000000000000 ) ;
#11840 = ORIENTED_EDGE ( 'NONE', *, *, #5845, .T. ) ;
#11841 = DIRECTION ( 'NONE',  ( -1.000000000000000000, 0.000000000000000000, 0.000000000000000000 ) ) ;
#11842 = CARTESIAN_POINT ( 'NONE',  ( -5.365059087799948223, 7.384370330706355290, 7.333165578109188232 ) ) ;
#11843 = EDGE_CURVE ( 'NONE', #556, #13484, #10937, .T. ) ;
#11844 = ADVANCED_FACE ( 'NONE', ( #18408 ), #7057, .F. ) ;
#11845 = CARTESIAN_POINT ( 'NONE',  ( -21.13207267780287069, -38.32709852940855910, 12.00000000000000000 ) ) ;
#11846 = LINE ( 'NONE', #17961, #12938 ) ;
#11847 = ORIENTED_EDGE ( 'NONE', *, *, #23057, .T. ) ;
#11848 = AXIS2_PLACEMENT_3D ( 'NONE', #9805, #22428, #3754 ) ;
#11849 = AXIS2_PLACEMENT_3D ( 'NONE', #7540, #11195, #13275 ) ;
#11850 = ORIENTED_EDGE ( 'NONE', *, *, #13056, .T. ) ;
#11851 = DIRECTION ( 'NONE',  ( 1.000000000000000000, -1.776356839400250465E-15, 0.000000000000000000 ) ) ;
#11852 = TOROIDAL_SURFACE ( 'NONE', #20457, 14.02592346138681201, 0.2999999999999999334 ) ;
#11853 = DIRECTION ( 'NONE',  ( 1.000000000000000000, 0.000000000000000000, 0.000000000000000000 ) ) ;
#11854 = VERTEX_POINT ( 'NONE', #9001 ) ;
#11855 = DIRECTION ( 'NONE',  ( 0.000000000000000000, -1.000000000000000000, 0.000000000000000000 ) ) ;
#11856 = CARTESIAN_POINT ( 'NONE',  ( 0.000000000000000000, 0.000000000000000000, 12.00000000000000000 ) ) ;
#11857 = VERTEX_POINT ( 'NONE', #1705 ) ;
#11858 = CARTESIAN_POINT ( 'NONE',  ( -2.024999999999999911, 45.00000000000000000, -3.000000000000000000 ) ) ;
#11859 = AXIS2_PLACEMENT_3D ( 'NONE', #20324, #18373, #1668 ) ;
#11860 = EDGE_CURVE ( 'NONE', #14197, #12486, #21959, .T. ) ;
#11861 = ORIENTED_EDGE ( 'NONE', *, *, #11746, .F. ) ;
#11862 = DIRECTION ( 'NONE',  ( 0.000000000000000000, 0.000000000000000000, -1.000000000000000000 ) ) ;
#11863 = FACE_OUTER_BOUND ( 'NONE', #11245, .T. ) ;
#11864 = CARTESIAN_POINT ( 'NONE',  ( 3.890962118697714531E-15, 15.50000000000000000, 19.70000000000000284 ) ) ;
#11865 = PRODUCT_DEFINITION_CONTEXT ( 'detailed design', #13382, 'design' ) ;
#11866 = AXIS2_PLACEMENT_3D ( 'NONE', #11728, #19574, #19341 ) ;
#11867 = CARTESIAN_POINT ( 'NONE',  ( 18.50000000000000000, 2.265596578422603396E-15, 0.000000000000000000 ) ) ;
#11868 = ORIENTED_EDGE ( 'NONE', *, *, #5896, .F. ) ;
#11869 = CARTESIAN_POINT ( 'NONE',  ( 69.63636363636364024, 4.172000000000015696, 0.000000000000000000 ) ) ;
#11870 = CARTESIAN_POINT ( 'NONE',  ( 0.000000000000000000, 0.000000000000000000, 0.000000000000000000 ) ) ;
#11871 = EDGE_CURVE ( 'NONE', #21144, #18515, #20760, .T. ) ;
#11872 = CARTESIAN_POINT ( 'NONE',  ( 42.00000000000000000, 3.999999999999987121, 10.49999999999999822 ) ) ;
#11873 = EDGE_LOOP ( 'NONE', ( #18778, #9831, #17182, #4576, #12270 ) ) ;
#11874 = EDGE_CURVE ( 'NONE', #3246, #7962, #20360, .T. ) ;
#11875 = CIRCLE ( 'NONE', #2087, 11.68650000001168898 ) ;
#11876 = ORIENTED_EDGE ( 'NONE', *, *, #8038, .T. ) ;
#11877 = CARTESIAN_POINT ( 'NONE',  ( 7.685661446561619314, 5.583959896779020049, 4.259589141758143960 ) ) ;
#11878 = ORIENTED_EDGE ( 'NONE', *, *, #9412, .T. ) ;
#11879 = VECTOR ( 'NONE', #15466, 1000.000000000000000 ) ;
#11880 = EDGE_LOOP ( 'NONE', ( #4435, #13801, #19640, #4326, #521 ) ) ;
#11881 = AXIS2_PLACEMENT_3D ( 'NONE', #3308, #18200, #1493 ) ;
#11882 = EDGE_LOOP ( 'NONE', ( #3328, #11735, #15523, #5884, #8376 ) ) ;
#11883 = CARTESIAN_POINT ( 'NONE',  ( -23.97499999999999787, 29.50000000000000000, -3.000000000000000000 ) ) ;
#11884 = CARTESIAN_POINT ( 'NONE',  ( -2.682529543900285862, 8.255977015246234174, -3.233165578109188587 ) ) ;
#11885 = CARTESIAN_POINT ( 'NONE',  ( -9.500000000000000000, -6.482511860946779655E-13, 8.206742014460234103 ) ) ;
#11886 = VERTEX_POINT ( 'NONE', #5479 ) ;
#11887 = DIRECTION ( 'NONE',  ( 0.000000000000000000, 0.000000000000000000, -1.000000000000000000 ) ) ;
#11888 = DIRECTION ( 'NONE',  ( -0.000000000000000000, -0.000000000000000000, -1.000000000000000000 ) ) ;
#11889 = CARTESIAN_POINT ( 'NONE',  ( 0.000000000000000000, 1.102182119232617714E-15, -9.000000000000000000 ) ) ;
#11890 = DIRECTION ( 'NONE',  ( -0.000000000000000000, -0.000000000000000000, 1.000000000000000000 ) ) ;
#11891 = VERTEX_POINT ( 'NONE', #12902 ) ;
#11892 = CARTESIAN_POINT ( 'NONE',  ( 11.50000000000000000, 12.02595010061954461, 13.22467954916291433 ) ) ;
#11893 = LINE ( 'NONE', #17999, #23904 ) ;
#11894 = VECTOR ( 'NONE', #5752, 1000.000000000000000 ) ;
#11895 = ORIENTED_EDGE ( 'NONE', *, *, #20043, .T. ) ;
#11896 = CARTESIAN_POINT ( 'NONE',  ( -39.99999999999999289, -29.50000000000001066, 27.00000000000000000 ) ) ;
#11897 = CARTESIAN_POINT ( 'NONE',  ( 35.99999999999999289, 50.99999999999999289, 0.5000000000000000000 ) ) ;
#11898 = AXIS2_PLACEMENT_3D ( 'NONE', #12361, #14077, #13842 ) ;
#11899 = CARTESIAN_POINT ( 'NONE',  ( 17.59041996266972063, -9.500503876990118002, 0.4759723220310708713 ) ) ;
#11900 = DIRECTION ( 'NONE',  ( -0.000000000000000000, -0.000000000000000000, -1.000000000000000000 ) ) ;
#11901 = CARTESIAN_POINT ( 'NONE',  ( -8.680847955710813579, -2.820578480814257549, -9.733165578109186811 ) ) ;
#11902 = EDGE_CURVE ( 'NONE', #16743, #4095, #116, .T. ) ;
#11903 = FACE_OUTER_BOUND ( 'NONE', #13278, .T. ) ;
#11904 = ORIENTED_EDGE ( 'NONE', *, *, #13238, .T. ) ;
#11905 = CARTESIAN_POINT ( 'NONE',  ( 5.365059087798938364, 7.384370330707087149, 10.93316557810918788 ) ) ;
#11906 = VECTOR ( 'NONE', #15433, 1000.000000000000000 ) ;
#11907 = EDGE_LOOP ( 'NONE', ( #20348, #18711 ) ) ;
#11908 = CARTESIAN_POINT ( 'NONE',  ( 1358.749511928808488, 1745.903857496118462, 48.72831690717735853 ) ) ;
#11909 = AXIS2_PLACEMENT_3D ( 'NONE', #19781, #16328, #16571 ) ;
#11910 = EDGE_LOOP ( 'NONE', ( #20323, #16082, #14342, #20789 ) ) ;
#11911 = DIRECTION ( 'NONE',  ( -0.000000000000000000, -0.000000000000000000, 1.000000000000000000 ) ) ;
#11912 = CARTESIAN_POINT ( 'NONE',  ( 71.67068093254673045, 5.000000000000015099, 0.000000000000000000 ) ) ;
#11913 = AXIS2_PLACEMENT_3D ( 'NONE', #10226, #3057, #10477 ) ;
#11914 = AXIS2_PLACEMENT_3D ( 'NONE', #17716, #1016, #2961 ) ;
#11915 = CYLINDRICAL_SURFACE ( 'NONE', #5998, 1.999999999999994449 ) ;
#11916 = CYLINDRICAL_SURFACE ( 'NONE', #627, 11.00000000000000711 ) ;
#11917 = CARTESIAN_POINT ( 'NONE',  ( -5.871322893123449127, -8.081182679344781405, 6.506742014460233925 ) ) ;
#11918 = ADVANCED_FACE ( 'NONE', ( #7407 ), #2437, .F. ) ;
#11919 = DIRECTION ( 'NONE',  ( 0.000000000000000000, 1.000000000000000000, 0.000000000000000000 ) ) ;
#11920 = CARTESIAN_POINT ( 'NONE',  ( 0.000000000000000000, 15.50000000000000000, 7.700000000000001954 ) ) ;
#11921 = ADVANCED_FACE ( 'NONE', ( #5602 ), #1660, .F. ) ;
#11922 = CARTESIAN_POINT ( 'NONE',  ( 23.00000000000000000, -13.61176534793449200, 10.13961790095610560 ) ) ;
#11923 = VERTEX_POINT ( 'NONE', #5728 ) ;
#11924 = AXIS2_PLACEMENT_3D ( 'NONE', #325, #16768, #15168 ) ;
#11925 = DIRECTION ( 'NONE',  ( 0.000000000000000000, 0.000000000000000000, -1.000000000000000000 ) ) ;
#11926 = FACE_OUTER_BOUND ( 'NONE', #21088, .T. ) ;
#11927 = CARTESIAN_POINT ( 'NONE',  ( 35.99999999999999289, -51.00000000000000711, 0.000000000000000000 ) ) ;
#11928 = AXIS2_PLACEMENT_3D ( 'NONE', #16158, #14085, #1052 ) ;
#11929 = EDGE_CURVE ( 'NONE', #18651, #1630, #17051, .T. ) ;
#11930 = DIRECTION ( 'NONE',  ( -0.000000000000000000, -0.000000000000000000, 1.000000000000000000 ) ) ;
#11931 = EDGE_LOOP ( 'NONE', ( #5591, #21895 ) ) ;
#11932 = CARTESIAN_POINT ( 'NONE',  ( 5.871322893124553133, -8.081182679343980269, -12.90674201446023517 ) ) ;
#11933 = AXIS2_PLACEMENT_3D ( 'NONE', #22947, #5981, #2319 ) ;
#11934 = ORIENTED_EDGE ( 'NONE', *, *, #6741, .T. ) ;
#11935 = EDGE_LOOP ( 'NONE', ( #24072, #21042, #11739, #14021, #2854, #18956 ) ) ;
#11936 = CARTESIAN_POINT ( 'NONE',  ( -6.822232771736903637E-13, 9.988891130263535700, 10.55958914175814378 ) ) ;
#11937 = DIRECTION ( 'NONE',  ( 0.000000000000000000, -1.000000000000000000, 0.000000000000000000 ) ) ;
#11938 = ORIENTED_EDGE ( 'NONE', *, *, #20164, .F. ) ;
#11939 = CARTESIAN_POINT ( 'NONE',  ( -5.365059087798939252, -7.384370330707086261, -11.93316557810918965 ) ) ;
#11940 = DIRECTION ( 'NONE',  ( -1.000000000000000000, 0.000000000000000000, -0.000000000000000000 ) ) ;
#11941 = CARTESIAN_POINT ( 'NONE',  ( -9.500000000000000000, -6.482511860946779655E-13, 7.059589141758143782 ) ) ;
#11942 = CIRCLE ( 'NONE', #17803, 4.999999999999997335 ) ;
#11943 = B_SPLINE_CURVE_WITH_KNOTS ( 'NONE', 3,
 ( #5266, #5038, #12693, #5137, #8798, #12447, #1724, #20161 ),
 .UNSPECIFIED., .F., .F.,
 ( 4, 2, 2, 4 ),
 ( 0.000000000000000000, 0.001825626494867788573, 0.002738439742301682859, 0.003651252989735577145 ),
 .UNSPECIFIED. ) ;
#11944 = CARTESIAN_POINT ( 'NONE',  ( 15.00000000000000000, 5.618453542512190434E-15, -9.499999999999987566 ) ) ;
#11945 = DIRECTION ( 'NONE',  ( -1.000000000000000000, 0.000000000000000000, -0.000000000000000000 ) ) ;
#11946 = DIRECTION ( 'NONE',  ( 0.000000000000000000, 0.000000000000000000, 1.000000000000000000 ) ) ;
#11947 = EDGE_LOOP ( 'NONE', ( #8072, #4322 ) ) ;
#11948 = EDGE_CURVE ( 'NONE', #12416, #16460, #13977, .T. ) ;
#11949 = EDGE_CURVE ( 'NONE', #1117, #8434, #16073, .T. ) ;
#11950 = EDGE_LOOP ( 'NONE', ( #580, #26, #9962, #22787, #9999, #3104 ) ) ;
#11951 = DIRECTION ( 'NONE',  ( 0.000000000000000000, -1.000000000000000000, 0.000000000000000000 ) ) ;
#11952 = CARTESIAN_POINT ( 'NONE',  ( -7.313784335799641489, -5.723601837928314673, 12.24551935885542875 ) ) ;
#11953 = CARTESIAN_POINT ( 'NONE',  ( 2.935661446562616295, -9.035036904803758873, 11.65958914175814520 ) ) ;
#11954 = LINE ( 'NONE', #19422, #7936 ) ;
#11955 = CARTESIAN_POINT ( 'NONE',  ( 39.99999999999999289, 27.79189783386526358, 27.00000000000000000 ) ) ;
#11956 = ORIENTED_EDGE ( 'NONE', *, *, #20164, .T. ) ;
#11957 = CYLINDRICAL_SURFACE ( 'NONE', #17231, 9.500000000000000000 ) ;
#11958 = DIRECTION ( 'NONE',  ( 0.000000000000000000, 1.000000000000000000, 0.000000000000000000 ) ) ;
#11959 = ORIENTED_EDGE ( 'NONE', *, *, #7669, .T. ) ;
#11960 = CARTESIAN_POINT ( 'NONE',  ( 6.809999908187194197E-13, -9.988891130263535700, -4.706742014460233214 ) ) ;
#11961 = ORIENTED_EDGE ( 'NONE', *, *, #18944, .T. ) ;
#11962 = FACE_OUTER_BOUND ( 'NONE', #22011, .T. ) ;
#11963 = CARTESIAN_POINT ( 'NONE',  ( 2.682529543900284974, -8.255977015246234174, 10.23316557810918859 ) ) ;
#11964 = DIRECTION ( 'NONE',  ( 0.8757121056631640421, -0.4828336235133042775, 0.000000000000000000 ) ) ;
#11965 = FACE_BOUND ( 'NONE', #6475, .T. ) ;
#11966 = ORIENTED_EDGE ( 'NONE', *, *, #12674, .F. ) ;
#11967 = DIRECTION ( 'NONE',  ( -1.000000000000000000, -0.000000000000000000, -0.000000000000000000 ) ) ;
#11968 = ADVANCED_FACE ( 'NONE', ( #7764 ), #15922, .T. ) ;
#11969 = CARTESIAN_POINT ( 'NONE',  ( 7.685661446561619314, 5.583959896779020049, -9.406742014460235168 ) ) ;
#11970 = ORIENTED_EDGE ( 'NONE', *, *, #7916, .T. ) ;
#11971 = ORIENTED_EDGE ( 'NONE', *, *, #8938, .T. ) ;
#11972 = CARTESIAN_POINT ( 'NONE',  ( -1.322535313088504250, -9.023848918650378081, -12.38804728513980180 ) ) ;
#11973 = ADVANCED_FACE ( 'NONE', ( #2295 ), #5952, .F. ) ;
#11974 = EDGE_CURVE ( 'NONE', #15590, #3047, #4004, .T. ) ;
#11975 = CARTESIAN_POINT ( 'NONE',  ( 0.000000000000000000, 32.75000000000000000, 16.70000000000000284 ) ) ;
#11976 = ORIENTED_EDGE ( 'NONE', *, *, #16378, .F. ) ;
#11977 = ORIENTED_EDGE ( 'NONE', *, *, #15791, .T. ) ;
#11978 = CARTESIAN_POINT ( 'NONE',  ( 28.99999999999999645, 29.49999999999999645, 0.000000000000000000 ) ) ;
#11979 = DIRECTION ( 'NONE',  ( -0.000000000000000000, 0.000000000000000000, -1.000000000000000000 ) ) ;
#11980 = CARTESIAN_POINT ( 'NONE',  ( 40.00000000000000000, 28.80990663662251450, 12.00000000000000000 ) ) ;
#11981 = CARTESIAN_POINT ( 'NONE',  ( 20.85000000000000497, -16.67999999999999972, 13.50000000000000178 ) ) ;
#11982 = ORIENTED_EDGE ( 'NONE', *, *, #2341, .T. ) ;
#11983 = CARTESIAN_POINT ( 'NONE',  ( 62.36363636363636687, -4.172000000000000597, 0.000000000000000000 ) ) ;
#11984 = CARTESIAN_POINT ( 'NONE',  ( 0.000000000000000000, 15.03999999999999915, -25.00000000000000000 ) ) ;
#11985 = LINE ( 'NONE', #6644, #22446 ) ;
#11986 = ORIENTED_EDGE ( 'NONE', *, *, #16556, .F. ) ;
#11987 = CIRCLE ( 'NONE', #13557, 5.000000000000007994 ) ;
#11988 = ORIENTED_EDGE ( 'NONE', *, *, #14081, .F. ) ;
#11989 = CARTESIAN_POINT ( 'NONE',  ( 9.500000000000000000, 6.470877716354879437E-13, 8.059589141758143782 ) ) ;
#11990 = ORIENTED_EDGE ( 'NONE', *, *, #6826, .T. ) ;
#11991 = EDGE_CURVE ( 'NONE', #19009, #9993, #20607, .T. ) ;
#11992 = ORIENTED_EDGE ( 'NONE', *, *, #6127, .F. ) ;
#11993 = ORIENTED_EDGE ( 'NONE', *, *, #10044, .T. ) ;
#11994 = VERTEX_POINT ( 'NONE', #7648 ) ;
#11995 = DIRECTION ( 'NONE',  ( 0.000000000000000000, -1.000000000000000000, 0.000000000000000000 ) ) ;
#11996 = CARTESIAN_POINT ( 'NONE',  ( 5.365059087799946447, -7.384370330706356178, -6.333165578109187344 ) ) ;
#11997 = CARTESIAN_POINT ( 'NONE',  ( -14.99999999999999822, -0.3242076166095216316, -9.499999999999994671 ) ) ;
#11998 = FACE_OUTER_BOUND ( 'NONE', #21691, .T. ) ;
#11999 = ORIENTED_EDGE ( 'NONE', *, *, #9412, .F. ) ;
#12000 = CARTESIAN_POINT ( 'NONE',  ( -14.51962751333974033, -3.765689428759031010, 8.721787840009202597 ) ) ;
#12001 = LINE ( 'NONE', #10165, #20122 ) ;
#12002 = ADVANCED_FACE ( 'NONE', ( #2746 ), #21419, .F. ) ;
#12003 = CARTESIAN_POINT ( 'NONE',  ( 0.000000000000000000, -10.66755332433018744, -4.772587172891147311 ) ) ;
#12004 = EDGE_CURVE ( 'NONE', #15840, #4885, #9713, .T. ) ;
#12005 = CARTESIAN_POINT ( 'NONE',  ( -28.99999999999999645, 29.50000000000000000, 14.00000000000000178 ) ) ;
#12006 = ORIENTED_EDGE ( 'NONE', *, *, #17441, .T. ) ;
#12007 = CARTESIAN_POINT ( 'NONE',  ( -9.499999999999786837, -3.086737114213265354, -8.306742014460233747 ) ) ;
#12008 = CARTESIAN_POINT ( 'NONE',  ( -7.685661446561619314, -5.583959896779019161, 7.259589141758143960 ) ) ;
#12009 = ORIENTED_EDGE ( 'NONE', *, *, #2787, .T. ) ;
#12010 = LINE ( 'NONE', #4607, #22203 ) ;
#12011 = LINE ( 'NONE', #6552, #12908 ) ;
#12012 = CARTESIAN_POINT ( 'NONE',  ( 16.36913330654531507, -6.602951766536811817, 6.845624079409791563 ) ) ;
#12013 = CARTESIAN_POINT ( 'NONE',  ( -9.000000000000001776, 0.000000000000000000, 12.50000000000000000 ) ) ;
#12014 = CARTESIAN_POINT ( 'NONE',  ( -2.682529543899159208, -8.255977015246598327, -8.033165578109189298 ) ) ;
#12015 = DIRECTION ( 'NONE',  ( -1.000000000000000000, 0.000000000000000000, 0.000000000000000000 ) ) ;
#12016 = ORIENTED_EDGE ( 'NONE', *, *, #11182, .F. ) ;
#12017 = VERTEX_POINT ( 'NONE', #22555 ) ;
#12018 = CARTESIAN_POINT ( 'NONE',  ( -5.365059087798939252, -7.384370330707086261, 9.933165578109189653 ) ) ;
#12019 = ORIENTED_EDGE ( 'NONE', *, *, #15961, .T. ) ;
#12020 = EDGE_CURVE ( 'NONE', #3116, #1372, #6259, .T. ) ;
#12021 = LINE ( 'NONE', #19254, #5831 ) ;
#12022 = ORIENTED_EDGE ( 'NONE', *, *, #17522, .T. ) ;
#12023 = DIRECTION ( 'NONE',  ( -0.000000000000000000, -0.000000000000000000, 1.000000000000000000 ) ) ;
#12024 = CARTESIAN_POINT ( 'NONE',  ( 9.500000000000000000, 6.470877716354879437E-13, -12.05958914175814378 ) ) ;
#12025 = CARTESIAN_POINT ( 'NONE',  ( 2.844143524245955845, 8.539150930870759382, 99.97419428330140079 ) ) ;
#12026 = DIRECTION ( 'NONE',  ( -1.000000000000000000, -1.224606353822377258E-16, -0.000000000000000000 ) ) ;
#12027 = DIRECTION ( 'NONE',  ( 0.000000000000000000, 1.000000000000000000, 0.000000000000000000 ) ) ;
#12028 = AXIS2_PLACEMENT_3D ( 'NONE', #15691, #10070, #2654 ) ;
#12029 = EDGE_CURVE ( 'NONE', #6200, #2336, #12560, .T. ) ;
#12030 = ORIENTED_EDGE ( 'NONE', *, *, #63, .F. ) ;
#12031 = CARTESIAN_POINT ( 'NONE',  ( 15.00000000000000355, 15.50000000000000000, 16.70000000000000284 ) ) ;
#12032 = ADVANCED_FACE ( 'NONE', ( #6417 ), #897, .F. ) ;
#12033 = FACE_OUTER_BOUND ( 'NONE', #18048, .T. ) ;
#12034 = DIRECTION ( 'NONE',  ( 0.000000000000000000, 0.000000000000000000, -1.000000000000000000 ) ) ;
#12035 = ORIENTED_EDGE ( 'NONE', *, *, #2609, .T. ) ;
#12036 = DIRECTION ( 'NONE',  ( 1.000000000000000000, 1.224606353822377258E-16, 0.000000000000000000 ) ) ;
#12037 = DIRECTION ( 'NONE',  ( -1.000000000000000000, -1.224606353822377258E-16, -0.000000000000000000 ) ) ;
#12038 = CARTESIAN_POINT ( 'NONE',  ( 40.00000000000000000, -29.49999999999999645, 12.00000000000000000 ) ) ;
#12039 = DIRECTION ( 'NONE',  ( -1.000000000000000000, 0.000000000000000000, 0.000000000000000000 ) ) ;
#12040 = AXIS2_PLACEMENT_3D ( 'NONE', #19596, #23499, #1060 ) ;
#12041 = VERTEX_POINT ( 'NONE', #4597 ) ;
#12042 = CARTESIAN_POINT ( 'NONE',  ( 8.680847955710813579, 2.820578480814259326, -4.733165578109188587 ) ) ;
#12043 = ORIENTED_EDGE ( 'NONE', *, *, #6741, .F. ) ;
#12044 = ORIENTED_EDGE ( 'NONE', *, *, #23556, .F. ) ;
#12045 = CARTESIAN_POINT ( 'NONE',  ( -2.935661446562617183, 9.035036904803758873, 6.659589141758144315 ) ) ;
#12046 = CARTESIAN_POINT ( 'NONE',  ( 9.499999999999790390, 3.086737114213260025, 11.30674201446023019 ) ) ;
#12047 = ORIENTED_EDGE ( 'NONE', *, *, #14862, .F. ) ;
#12048 = AXIS2_PLACEMENT_3D ( 'NONE', #15349, #19279, #11937 ) ;
#12049 = CARTESIAN_POINT ( 'NONE',  ( 42.00000000000000000, 26.82133436441678853, 11.00000000000000000 ) ) ;
#12050 = CIRCLE ( 'NONE', #8548, 5.099999999999996980 ) ;
#12051 = DIRECTION ( 'NONE',  ( -0.000000000000000000, -0.000000000000000000, -1.000000000000000000 ) ) ;
#12052 = ADVANCED_FACE ( 'NONE', ( #11998 ), #11290, .T. ) ;
#12053 = CARTESIAN_POINT ( 'NONE',  ( -2.000000000000000000, 0.000000000000000000, 5.499999999999997335 ) ) ;
#12054 = CARTESIAN_POINT ( 'NONE',  ( 88.54545454545454675, -4.172000000000000597, 0.000000000000000000 ) ) ;
#12055 = CARTESIAN_POINT ( 'NONE',  ( 4.810877257134754004, -7.548248927254270768, -12.49999999999999822 ) ) ;
#12056 = ADVANCED_FACE ( 'NONE', ( #23267 ), #5976, .T. ) ;
#12057 = CYLINDRICAL_SURFACE ( 'NONE', #12141, 9.500000000000000000 ) ;
#12058 = ADVANCED_FACE ( 'NONE', ( #18347 ), #21890, .T. ) ;
#12059 = ORIENTED_EDGE ( 'NONE', *, *, #11437, .T. ) ;
#12060 = ORIENTED_EDGE ( 'NONE', *, *, #10147, .F. ) ;
#12061 = CARTESIAN_POINT ( 'NONE',  ( 41.00000000000000000, -6.000000000000015099, 9.500000000000000000 ) ) ;
#12062 = DIRECTION ( 'NONE',  ( 0.000000000000000000, 0.000000000000000000, 1.000000000000000000 ) ) ;
#12063 = CARTESIAN_POINT ( 'NONE',  ( -39.99999999999999289, -29.50000000000001066, 27.00000000000000000 ) ) ;
#12064 = CARTESIAN_POINT ( 'NONE',  ( -29.00000000000000000, -29.49999999999999645, 0.000000000000000000 ) ) ;
#12065 = VECTOR ( 'NONE', #11461, 1000.000000000000000 ) ;
#12066 = DIRECTION ( 'NONE',  ( -1.000000000000000000, -0.000000000000000000, 0.000000000000000000 ) ) ;
#12067 = ORIENTED_EDGE ( 'NONE', *, *, #10422, .T. ) ;
#12068 = CARTESIAN_POINT ( 'NONE',  ( 3.890962118697714531E-15, 15.50000000000000000, 7.700000000000001954 ) ) ;
#12069 = VERTEX_POINT ( 'NONE', #12607 ) ;
#12070 = DIRECTION ( 'NONE',  ( -1.000000000000000000, 0.000000000000000000, 0.000000000000000000 ) ) ;
#12071 = ORIENTED_EDGE ( 'NONE', *, *, #20741, .T. ) ;
#12072 = DIRECTION ( 'NONE',  ( 1.000000000000000000, 0.000000000000000000, 0.000000000000000000 ) ) ;
#12073 = CARTESIAN_POINT ( 'NONE',  ( -7.022953521755574080, 5.102474405759713783, 5.433165578109188765 ) ) ;
#12074 = EDGE_CURVE ( 'NONE', #6367, #18342, #13371, .T. ) ;
#12075 = FACE_OUTER_BOUND ( 'NONE', #11947, .T. ) ;
#12076 = LINE ( 'NONE', #19549, #8338 ) ;
#12077 = CARTESIAN_POINT ( 'NONE',  ( 34.10000000000001563, -29.50000000000000711, 27.00000000000000000 ) ) ;
#12078 = EDGE_CURVE ( 'NONE', #10129, #9582, #16027, .T. ) ;
#12079 = CARTESIAN_POINT ( 'NONE',  ( -6.249999999999999112, -10.82531754730548279, -2.500000000000000000 ) ) ;
#12080 = VERTEX_POINT ( 'NONE', #23496 ) ;
#12081 = CONTEXT_DEPENDENT_SHAPE_REPRESENTATION ( #5893, #5369 ) ;
#12082 = EDGE_LOOP ( 'NONE', ( #22594, #21044 ) ) ;
#12083 = DIRECTION ( 'NONE',  ( 0.000000000000000000, 0.000000000000000000, 1.000000000000000000 ) ) ;
#12084 = CARTESIAN_POINT ( 'NONE',  ( -9.500000000000211386, 3.086737114211961064, -12.10674201446023091 ) ) ;
#12085 = VERTEX_POINT ( 'NONE', #8939 ) ;
#12086 = CARTESIAN_POINT ( 'NONE',  ( 2.511895845244684455, -8.709941883493257819, -12.46858854093511049 ) ) ;
#12087 = FACE_OUTER_BOUND ( 'NONE', #18668, .T. ) ;
#12088 = ORIENTED_EDGE ( 'NONE', *, *, #3093, .F. ) ;
#12089 = CARTESIAN_POINT ( 'NONE',  ( -42.00000000000000000, 25.22443390181683043, -1.500000000000000000 ) ) ;
#12090 = ORIENTED_EDGE ( 'NONE', *, *, #23900, .F. ) ;
#12091 = LINE ( 'NONE', #23472, #4083 ) ;
#12092 = PLANE ( 'NONE',  #13720 ) ;
#12093 = DIRECTION ( 'NONE',  ( 1.000000000000000000, 0.000000000000000000, 0.000000000000000000 ) ) ;
#12094 = CARTESIAN_POINT ( 'NONE',  ( -14.99999999999999822, 0.000000000000000000, 27.00000000000000000 ) ) ;
#12095 = LINE ( 'NONE', #6396, #1384 ) ;
#12096 = VECTOR ( 'NONE', #20346, 1000.000000000000000 ) ;
#12097 = EDGE_LOOP ( 'NONE', ( #10468, #18960, #11208, #785 ) ) ;
#12098 = CARTESIAN_POINT ( 'NONE',  ( -1.749335460928132413, -9.337549220493531976, -3.500000000000076383 ) ) ;
#12099 = CARTESIAN_POINT ( 'NONE',  ( -34.00000000000000000, 5.999999999999999112, 12.00000000000000000 ) ) ;
#12100 = CYLINDRICAL_SURFACE ( 'NONE', #10357, 3.000000000000002665 ) ;
#12101 = CIRCLE ( 'NONE', #15620, 5.000000000000007994 ) ;
#12102 = CARTESIAN_POINT ( 'NONE',  ( -2.935661446561384391, -9.035036904804158553, 7.459589141758144137 ) ) ;
#12103 = EDGE_LOOP ( 'NONE', ( #19722, #16424, #14960, #9393 ) ) ;
#12104 = ADVANCED_FACE ( 'NONE', ( #9064 ), #4812, .T. ) ;
#12105 = VERTEX_POINT ( 'NONE', #14429 ) ;
#12106 = EDGE_CURVE ( 'NONE', #2619, #8063, #15308, .T. ) ;
#12107 = ORIENTED_EDGE ( 'NONE', *, *, #14116, .T. ) ;
#12108 = ORIENTED_EDGE ( 'NONE', *, *, #21912, .F. ) ;
#12109 = ORIENTED_EDGE ( 'NONE', *, *, #1978, .F. ) ;
#12110 = DIRECTION ( 'NONE',  ( 0.000000000000000000, 0.000000000000000000, 1.000000000000000000 ) ) ;
#12111 = CARTESIAN_POINT ( 'NONE',  ( -21.84999999999999787, 16.67999999999985405, 12.00000000000000000 ) ) ;
#12112 = CARTESIAN_POINT ( 'NONE',  ( 23.00000000000000000, -1.934484387512043435, 14.08058594723506474 ) ) ;
#12113 = VECTOR ( 'NONE', #18009, 1000.000000000000000 ) ;
#12114 = ORIENTED_EDGE ( 'NONE', *, *, #2324, .T. ) ;
#12115 = DIRECTION ( 'NONE',  ( -1.000000000000000000, 0.000000000000000000, 0.000000000000000000 ) ) ;
#12116 =( REPRESENTATION_RELATIONSHIP ('NONE','NONE', #21748, #12815 ) REPRESENTATION_RELATIONSHIP_WITH_TRANSFORMATION ( #5777 )SHAPE_REPRESENTATION_RELATIONSHIP( ) );
#12117 = B_SPLINE_CURVE_WITH_KNOTS ( 'NONE', 3,
 ( #2756, #8225, #12266, #21681, #2646, #1299, #12385, #19737 ),
 .UNSPECIFIED., .F., .F.,
 ( 4, 2, 2, 4 ),
 ( 0.003892319173193281752, 0.004864202078960306805, 0.005836084984727332725, 0.007779850796261384566 ),
 .UNSPECIFIED. ) ;
#12118 = CIRCLE ( 'NONE', #9006, 5.000000000000007994 ) ;
#12119 = FACE_OUTER_BOUND ( 'NONE', #21618, .T. ) ;
#12120 = CIRCLE ( 'NONE', #20326, 5.000000000000007994 ) ;
#12121 = VERTEX_POINT ( 'NONE', #21543 ) ;
#12122 = CARTESIAN_POINT ( 'NONE',  ( 6.809999908187194197E-13, -9.988891130263535700, -8.706742014460232326 ) ) ;
#12123 = DIRECTION ( 'NONE',  ( -1.000000000000000000, 0.000000000000000000, -0.000000000000000000 ) ) ;
#12124 = CARTESIAN_POINT ( 'NONE',  ( 6.809999908187194197E-13, -9.988891130263535700, 6.706742014460232326 ) ) ;
#12125 = ORIENTED_EDGE ( 'NONE', *, *, #21365, .F. ) ;
#12126 = CARTESIAN_POINT ( 'NONE',  ( 0.000000000000000000, -45.00000000000000000, 27.00000000000000000 ) ) ;
#12127 = DIRECTION ( 'NONE',  ( 0.000000000000000000, 0.000000000000000000, 1.000000000000000000 ) ) ;
#12128 = CARTESIAN_POINT ( 'NONE',  ( -17.25000000000000000, 15.50000000000000000, 16.70000000000000284 ) ) ;
#12129 = EDGE_CURVE ( 'NONE', #10256, #18213, #12579, .T. ) ;
#12130 = FACE_OUTER_BOUND ( 'NONE', #11491, .T. ) ;
#12131 = CARTESIAN_POINT ( 'NONE',  ( 8.680847955711199049, -2.820578480813074496, -8.533165578109187521 ) ) ;
#12132 = ADVANCED_FACE ( 'NONE', ( #6653 ), #21782, .F. ) ;
#12133 = LINE ( 'NONE', #8494, #15204 ) ;
#12134 = ORIENTED_EDGE ( 'NONE', *, *, #15234, .F. ) ;
#12135 = ORIENTED_EDGE ( 'NONE', *, *, #21700, .T. ) ;
#12136 = CIRCLE ( 'NONE', #13367, 9.999999999999998224 ) ;
#12137 = EDGE_CURVE ( 'NONE', #16240, #10789, #1701, .T. ) ;
#12138 = ADVANCED_FACE ( 'NONE', ( #14200 ), #14558, .T. ) ;
#12139 = PRODUCT_DEFINITION_SHAPE ( 'NONE', 'NONE',  #8694 ) ;
#12140 = ADVANCED_FACE ( 'NONE', ( #5305 ), #16859, .F. ) ;
#12141 = AXIS2_PLACEMENT_3D ( 'NONE', #4773, #10588, #19891 ) ;
#12142 = VERTEX_POINT ( 'NONE', #17883 ) ;
#12143 = APPLICATION_PROTOCOL_DEFINITION ( 'draft international standard', 'automotive_design', 1998, #4825 ) ;
#12144 = CARTESIAN_POINT ( 'NONE',  ( -2.935661446562617183, 9.035036904803758873, -11.80674201446023375 ) ) ;
#12145 = ORIENTED_EDGE ( 'NONE', *, *, #12749, .T. ) ;
#12146 = CARTESIAN_POINT ( 'NONE',  ( 0.000000000000000000, 0.000000000000000000, -12.00000000000000000 ) ) ;
#12147 = CARTESIAN_POINT ( 'NONE',  ( 2.935661446562616295, -9.035036904803758873, -11.65958914175814520 ) ) ;
#12148 = CARTESIAN_POINT ( 'NONE',  ( -0.7838698549262745896, 8.967904882329030158, 101.9025279484636428 ) ) ;
#12149 = CARTESIAN_POINT ( 'NONE',  ( 66.14750088563508257, 5.000000000000025757, 6.123233995736788962E-16 ) ) ;
#12150 = ORIENTED_EDGE ( 'NONE', *, *, #24056, .T. ) ;
#12151 = ORIENTED_EDGE ( 'NONE', *, *, #8641, .T. ) ;
#12152 = CARTESIAN_POINT ( 'NONE',  ( 0.000000000000000000, -45.00000000000000000, -3.000000000000000000 ) ) ;
#12153 = CIRCLE ( 'NONE', #13712, 1.999999999999994449 ) ;
#12154 = AXIS2_PLACEMENT_3D ( 'NONE', #8441, #3079, #10502 ) ;
#12155 = DIRECTION ( 'NONE',  ( -0.000000000000000000, -1.000000000000000000, -0.000000000000000000 ) ) ;
#12156 = ORIENTED_EDGE ( 'NONE', *, *, #4500, .F. ) ;
#12157 = DIRECTION ( 'NONE',  ( -0.000000000000000000, -0.000000000000000000, -1.000000000000000000 ) ) ;
#12158 = VERTEX_POINT ( 'NONE', #3352 ) ;
#12159 = CARTESIAN_POINT ( 'NONE',  ( 0.000000000000000000, 0.000000000000000000, 0.000000000000000000 ) ) ;
#12160 = CONICAL_SURFACE ( 'NONE', #7118, 5.000000000000007994, 0.9599310885968855844 ) ;
#12161 = DIRECTION ( 'NONE',  ( -0.000000000000000000, -0.000000000000000000, 1.000000000000000000 ) ) ;
#12162 = VECTOR ( 'NONE', #22617, 1000.000000000000000 ) ;
#12163 = EDGE_CURVE ( 'NONE', #8481, #1117, #18055, .T. ) ;
#12164 = AXIS2_PLACEMENT_3D ( 'NONE', #2824, #8906, #6857 ) ;
#12165 = DIRECTION ( 'NONE',  ( 0.000000000000000000, -1.000000000000000000, 0.000000000000000000 ) ) ;
#12166 = ORIENTED_EDGE ( 'NONE', *, *, #17355, .T. ) ;
#12167 =( BOUNDED_CURVE ( )  B_SPLINE_CURVE ( 2, ( #18224, #18106, #8816, #16261, #16141, #6882, #23718 ),
 .UNSPECIFIED., .F., .F. ) 
 B_SPLINE_CURVE_WITH_KNOTS ( ( 3, 2, 2, 3 ),
 ( 0.8000000000000000444, 0.8199999999999999512, 0.8399999999999999689, 0.8558632199373886751 ),
 .UNSPECIFIED. ) 
 CURVE ( )  GEOMETRIC_REPRESENTATION_ITEM ( )  RATIONAL_B_SPLINE_CURVE ( ( 1.000000000000000000, 0.9510565162951535312, 1.000000000000000000, 0.9510565162951535312, 1.000000000000000000, 0.9611799376744010193, 0.9839409940142134214 ) ) 
 REPRESENTATION_ITEM ( '' )  );
#12168 = ADVANCED_FACE ( 'NONE', ( #3107 ), #12482, .F. ) ;
#12169 = ORIENTED_EDGE ( 'NONE', *, *, #16694, .T. ) ;
#12170 = VERTEX_POINT ( 'NONE', #3224 ) ;
#12171 = CARTESIAN_POINT ( 'NONE',  ( -6.822232771736903637E-13, 9.988891130263535700, 4.559589141758142894 ) ) ;
#12172 = PLANE ( 'NONE',  #22583 ) ;
#12173 = EDGE_CURVE ( 'NONE', #1863, #8263, #23836, .T. ) ;
#12174 = EDGE_CURVE ( 'NONE', #21535, #19925, #13759, .T. ) ;
#12175 = VERTEX_POINT ( 'NONE', #20553 ) ;
#12176 =( NAMED_UNIT ( * ) SI_UNIT ( $, .STERADIAN. ) SOLID_ANGLE_UNIT ( ) );
#12177 = LINE ( 'NONE', #4535, #9536 ) ;
#12178 = AXIS2_PLACEMENT_3D ( 'NONE', #3262, #8248, #15707 ) ;
#12179 = VECTOR ( 'NONE', #17332, 1000.000000000000000 ) ;
#12180 = DIRECTION ( 'NONE',  ( -1.000000000000000000, 0.000000000000000000, 0.000000000000000000 ) ) ;
#12181 = CIRCLE ( 'NONE', #18429, 11.00000000000000711 ) ;
#12182 = VECTOR ( 'NONE', #1828, 1000.000000000000000 ) ;
#12183 = AXIS2_PLACEMENT_3D ( 'NONE', #5465, #9111, #8981 ) ;
#12184 = EDGE_LOOP ( 'NONE', ( #3989, #4352, #11837 ) ) ;
#12185 = TOROIDAL_SURFACE ( 'NONE', #121, 10.00000000000000533, 1.000000000000000000 ) ;
#12186 = DIRECTION ( 'NONE',  ( 0.8757121056631640421, 0.4828336235133042775, 0.000000000000000000 ) ) ;
#12187 = CYLINDRICAL_SURFACE ( 'NONE', #19193, 5.099999999999996980 ) ;
#12188 = AXIS2_PLACEMENT_3D ( 'NONE', #13717, #23811, #16249 ) ;
#12189 = VERTEX_POINT ( 'NONE', #20298 ) ;
#12190 = DIRECTION ( 'NONE',  ( 1.000000000000000000, 0.000000000000000000, 0.000000000000000000 ) ) ;
#12191 = ORIENTED_EDGE ( 'NONE', *, *, #1078, .T. ) ;
#12192 = CARTESIAN_POINT ( 'NONE',  ( 2.024999999999999911, -45.00000000000000000, -27.00000000000000000 ) ) ;
#12193 = SURFACE_SIDE_STYLE ('',( #16339 ) ) ;
#12194 = DIRECTION ( 'NONE',  ( -1.000000000000000000, -0.000000000000000000, -0.000000000000000000 ) ) ;
#12195 = DIRECTION ( 'NONE',  ( -1.000000000000000000, 0.000000000000000000, 0.000000000000000000 ) ) ;
#12196 = CIRCLE ( 'NONE', #15302, 15.00000000000000000 ) ;
#12197 = CARTESIAN_POINT ( 'NONE',  ( 23.00000000000000000, 5.823083658124710738, 12.96521604808350503 ) ) ;
#12198 = ORIENTED_EDGE ( 'NONE', *, *, #3412, .F. ) ;
#12199 = AXIS2_PLACEMENT_3D ( 'NONE', #9970, #15581, #15470 ) ;
#12200 = AXIS2_PLACEMENT_3D ( 'NONE', #16161, #14319, #17992 ) ;
#12201 = CARTESIAN_POINT ( 'NONE',  ( 0.000000000000000000, -14.96647757894464270, 7.750000000000000000 ) ) ;
#12202 = CIRCLE ( 'NONE', #9080, 5.000000000000007994 ) ;
#12203 = VERTEX_POINT ( 'NONE', #18706 ) ;
#12204 = DIRECTION ( 'NONE',  ( 0.8571673007021116675, 0.000000000000000000, 0.5150380749100552658 ) ) ;
#12205 = VERTEX_POINT ( 'NONE', #9654 ) ;
#12206 = AXIS2_PLACEMENT_3D ( 'NONE', #18585, #18941, #3922 ) ;
#12207 = DIRECTION ( 'NONE',  ( -0.000000000000000000, -0.000000000000000000, 1.000000000000000000 ) ) ;
#12208 = EDGE_CURVE ( 'NONE', #7332, #13485, #1155, .T. ) ;
#12209 = CONICAL_SURFACE ( 'NONE', #1706, 4.172000000000008590, 0.9599310885968742602 ) ;
#12210 = DIRECTION ( 'NONE',  ( -1.000000000000000000, 0.000000000000000000, -0.000000000000000000 ) ) ;
#12211 = CARTESIAN_POINT ( 'NONE',  ( -1.029124893018731811E-15, -45.00000000000000000, 1.201721238055119212 ) ) ;
#12212 = DIRECTION ( 'NONE',  ( -0.000000000000000000, -0.000000000000000000, -1.000000000000000000 ) ) ;
#12213 = CARTESIAN_POINT ( 'NONE',  ( 66.72727272727273373, 4.172000000000015696, 0.000000000000000000 ) ) ;
#12214 = VECTOR ( 'NONE', #2445, 1000.000000000000000 ) ;
#12215 = CONTEXT_DEPENDENT_SHAPE_REPRESENTATION ( #9302, #18812 ) ;
#12216 = VERTEX_POINT ( 'NONE', #7355 ) ;
#12217 = CARTESIAN_POINT ( 'NONE',  ( 33.99999999999998579, -6.000000000000013323, 11.00000000000000000 ) ) ;
#12218 = CIRCLE ( 'NONE', #8699, 1.000000000000001998 ) ;
#12219 = ORIENTED_EDGE ( 'NONE', *, *, #4398, .T. ) ;
#12220 = CIRCLE ( 'NONE', #17685, 1.000000000000000000 ) ;
#12221 = ORIENTED_EDGE ( 'NONE', *, *, #10179, .T. ) ;
#12222 = CIRCLE ( 'NONE', #21604, 4.172000000000008590 ) ;
#12223 = EDGE_CURVE ( 'NONE', #7988, #18527, #1876, .T. ) ;
#12224 = CARTESIAN_POINT ( 'NONE',  ( 9.301232020971124115, 6.335487896752474877E-13, 12.19876797902887233 ) ) ;
#12225 = VECTOR ( 'NONE', #12760, 1000.000000000000000 ) ;
#12226 = ORIENTED_EDGE ( 'NONE', *, *, #6041, .F. ) ;
#12227 = DIRECTION ( 'NONE',  ( -0.000000000000000000, -0.000000000000000000, -1.000000000000000000 ) ) ;
#12228 = CIRCLE ( 'NONE', #6411, 0.2999999999999999334 ) ;
#12229 = EDGE_CURVE ( 'NONE', #16185, #17812, #11397, .T. ) ;
#12230 = VERTEX_POINT ( 'NONE', #7704 ) ;
#12231 = CARTESIAN_POINT ( 'NONE',  ( 0.000000000000000000, 0.000000000000000000, 0.9999999999999940048 ) ) ;
#12232 = DIRECTION ( 'NONE',  ( -1.000000000000000000, -8.175701033892699531E-16, 0.000000000000000000 ) ) ;
#12233 = FACE_BOUND ( 'NONE', #2489, .T. ) ;
#12234 = DIRECTION ( 'NONE',  ( 0.000000000000000000, 0.000000000000000000, -1.000000000000000000 ) ) ;
#12235 = ADVANCED_FACE ( 'NONE', ( #22150 ), #14908, .T. ) ;
#12236 = DIRECTION ( 'NONE',  ( 1.000000000000000000, 0.000000000000000000, 0.000000000000000000 ) ) ;
#12237 = ORIENTED_EDGE ( 'NONE', *, *, #9315, .T. ) ;
#12238 = CARTESIAN_POINT ( 'NONE',  ( 9.324366623732823450E-16, 111.0000000000000000, 80.99999999999998579 ) ) ;
#12239 = CARTESIAN_POINT ( 'NONE',  ( 0.000000000000000000, 0.000000000000000000, 12.50000000000000000 ) ) ;
#12240 = FACE_OUTER_BOUND ( 'NONE', #22679, .T. ) ;
#12241 = CARTESIAN_POINT ( 'NONE',  ( 6.809999908187194197E-13, -9.988891130263535700, 7.559589141758143782 ) ) ;
#12242 = CIRCLE ( 'NONE', #11053, 4.172000000000008590 ) ;
#12243 = AXIS2_PLACEMENT_3D ( 'NONE', #20512, #1946, #9365 ) ;
#12244 = AXIS2_PLACEMENT_3D ( 'NONE', #24054, #14409, #14660 ) ;
#12245 = AXIS2_PLACEMENT_3D ( 'NONE', #7383, #9574, #7739 ) ;
#12246 = ORIENTED_EDGE ( 'NONE', *, *, #2709, .T. ) ;
#12247 = EDGE_LOOP ( 'NONE', ( #23617, #6660, #1610, #1716 ) ) ;
#12248 = EDGE_LOOP ( 'NONE', ( #4162, #19194, #22627, #10182 ) ) ;
#12249 = DIRECTION ( 'NONE',  ( 0.000000000000000000, 0.000000000000000000, 1.000000000000000000 ) ) ;
#12250 = DIRECTION ( 'NONE',  ( -1.000000000000000000, -1.224606353822377258E-16, -0.000000000000000000 ) ) ;
#12251 = DIRECTION ( 'NONE',  ( -0.000000000000000000, -0.000000000000000000, -1.000000000000000000 ) ) ;
#12252 = VERTEX_POINT ( 'NONE', #9399 ) ;
#12253 = DIRECTION ( 'NONE',  ( 0.000000000000000000, 0.000000000000000000, 1.000000000000000000 ) ) ;
#12254 = EDGE_CURVE ( 'NONE', #379, #8401, #6748, .T. ) ;
#12255 = DIRECTION ( 'NONE',  ( 0.000000000000000000, 0.000000000000000000, 1.000000000000000000 ) ) ;
#12256 = EDGE_LOOP ( 'NONE', ( #10527, #19562, #9990, #20596 ) ) ;
#12257 = CARTESIAN_POINT ( 'NONE',  ( -7.685661446561619314, -5.583959896779019161, -8.406742014460233392 ) ) ;
#12258 = DIRECTION ( 'NONE',  ( 0.000000000000000000, 0.5406408174555985546, -0.8412535328311806504 ) ) ;
#12259 = CIRCLE ( 'NONE', #1749, 8.000000000000003553 ) ;
#12260 = CYLINDRICAL_SURFACE ( 'NONE', #16473, 1.500000000000001332 ) ;
#12261 = EDGE_CURVE ( 'NONE', #17474, #15563, #10250, .T. ) ;
#12262 = EDGE_CURVE ( 'NONE', #4656, #14009, #18430, .T. ) ;
#12263 = DIRECTION ( 'NONE',  ( -1.000000000000000000, -1.224606353822377258E-16, -0.000000000000000000 ) ) ;
#12264 = DIRECTION ( 'NONE',  ( -0.000000000000000000, -0.000000000000000000, -1.000000000000000000 ) ) ;
#12265 = AXIS2_PLACEMENT_3D ( 'NONE', #9697, #17896, #1185 ) ;
#12266 = CARTESIAN_POINT ( 'NONE',  ( -14.98952570844870102, -0.6468970097546548059, 9.483487670324118213 ) ) ;
#12267 = DIRECTION ( 'NONE',  ( -1.000000000000000000, -0.000000000000000000, -0.000000000000000000 ) ) ;
#12268 = DIRECTION ( 'NONE',  ( -0.000000000000000000, -0.000000000000000000, -1.000000000000000000 ) ) ;
#12269 = AXIS2_PLACEMENT_3D ( 'NONE', #22409, #22172, #18151 ) ;
#12270 = ORIENTED_EDGE ( 'NONE', *, *, #7778, .F. ) ;
#12271 = LINE ( 'NONE', #15559, #19916 ) ;
#12272 = AXIS2_PLACEMENT_3D ( 'NONE', #24026, #14848, #5835 ) ;
#12273 = ORIENTED_EDGE ( 'NONE', *, *, #23363, .F. ) ;
#12274 = CARTESIAN_POINT ( 'NONE',  ( 7.022953521754877748, 5.102474405760673903, 6.833165578109188232 ) ) ;
#12275 = ORIENTED_EDGE ( 'NONE', *, *, #15108, .F. ) ;
#12276 = PRODUCT_CONTEXT ( 'NONE', #1971, 'mechanical' ) ;
#12277 = CARTESIAN_POINT ( 'NONE',  ( 0.000000000000000000, 0.000000000000000000, 0.9999999999999940048 ) ) ;
#12278 = ORIENTED_EDGE ( 'NONE', *, *, #1104, .T. ) ;
#12279 = DIRECTION ( 'NONE',  ( -1.000000000000000000, -1.224606353822377258E-16, -0.000000000000000000 ) ) ;
#12280 = CARTESIAN_POINT ( 'NONE',  ( 7.685661446561619314, 5.583959896779020049, -6.259589141758143960 ) ) ;
#12281 = PRODUCT_DEFINITION ( 'UNKNOWN', '', #4562, #22878 ) ;
#12282 = AXIS2_PLACEMENT_3D ( 'NONE', #9761, #19188, #20909 ) ;
#12283 = EDGE_CURVE ( 'NONE', #831, #20068, #13315, .T. ) ;
#12284 = AXIS2_PLACEMENT_3D ( 'NONE', #20877, #4167, #2685 ) ;
#12285 = CARTESIAN_POINT ( 'NONE',  ( -20.99999999999999645, 29.49999999999999645, 11.50000000000000000 ) ) ;
#12286 = DIRECTION ( 'NONE',  ( -0.000000000000000000, -0.000000000000000000, -1.000000000000000000 ) ) ;
#12287 = CARTESIAN_POINT ( 'NONE',  ( 29.00000000000000355, 29.50000000000000000, 27.00000000000000000 ) ) ;
#12288 = CIRCLE ( 'NONE', #1778, 5.099999999999996980 ) ;
#12289 = ORIENTED_EDGE ( 'NONE', *, *, #22772, .T. ) ;
#12290 = CONICAL_SURFACE ( 'NONE', #1779, 1.499999999999999556, 0.7853981633974457255 ) ;
#12291 = LINE ( 'NONE', #8512, #3999 ) ;
#12292 = ADVANCED_FACE ( 'NONE', ( #20783 ), #18825, .T. ) ;
#12293 = DIRECTION ( 'NONE',  ( 0.000000000000000000, 0.000000000000000000, 1.000000000000000000 ) ) ;
#12294 = EDGE_CURVE ( 'NONE', #20664, #5794, #14534, .T. ) ;
#12295 = CARTESIAN_POINT ( 'NONE',  ( -45.00000000000000000, -50.99999999999993605, 0.000000000000000000 ) ) ;
#12296 = DIRECTION ( 'NONE',  ( 0.000000000000000000, 0.000000000000000000, 1.000000000000000000 ) ) ;
#12297 = CARTESIAN_POINT ( 'NONE',  ( -10.00000000000000000, 0.000000000000000000, 0.000000000000000000 ) ) ;
#12298 = DIRECTION ( 'NONE',  ( -1.000000000000000000, 0.000000000000000000, 0.000000000000000000 ) ) ;
#12299 = ORIENTED_EDGE ( 'NONE', *, *, #6203, .T. ) ;
#12300 = CARTESIAN_POINT ( 'NONE',  ( 6.222797240145152671E-13, -9.127583699786111282, -4.133165578109187166 ) ) ;
#12301 = VERTEX_POINT ( 'NONE', #9539 ) ;
#12302 = AXIS2_PLACEMENT_3D ( 'NONE', #19408, #10227, #17689 ) ;
#12303 = EDGE_LOOP ( 'NONE', ( #17905, #13581, #11759, #14792 ) ) ;
#12304 = CARTESIAN_POINT ( 'NONE',  ( -5.871322893123450015, -8.081182679344781405, 3.359589141758143160 ) ) ;
#12305 = CARTESIAN_POINT ( 'NONE',  ( 5.871322893123449127, 8.081182679344781405, 5.506742014460233925 ) ) ;
#12306 = AXIS2_PLACEMENT_3D ( 'NONE', #23388, #6661, #14205 ) ;
#12307 = ORIENTED_EDGE ( 'NONE', *, *, #19908, .F. ) ;
#12308 =( NAMED_UNIT ( * ) PLANE_ANGLE_UNIT ( ) SI_UNIT ( $, .RADIAN. ) );
#12309 = AXIS2_PLACEMENT_3D ( 'NONE', #6264, #23481, #6531 ) ;
#12310 = DIRECTION ( 'NONE',  ( 0.000000000000000000, -1.000000000000000000, 0.000000000000000000 ) ) ;
#12311 = ORIENTED_EDGE ( 'NONE', *, *, #17813, .F. ) ;
#12312 = DIRECTION ( 'NONE',  ( -1.000000000000000000, 0.000000000000000000, 0.000000000000000000 ) ) ;
#12313 = EDGE_CURVE ( 'NONE', #13157, #15534, #18958, .T. ) ;
#12314 = DIRECTION ( 'NONE',  ( -0.000000000000000000, -0.000000000000000000, -1.000000000000000000 ) ) ;
#12315 = DIRECTION ( 'NONE',  ( -1.000000000000000000, 0.000000000000000000, 0.000000000000000000 ) ) ;
#12316 = CARTESIAN_POINT ( 'NONE',  ( -9.500000000000000000, 0.000000000000000000, 12.50000000000000000 ) ) ;
#12317 = VECTOR ( 'NONE', #7030, 1000.000000000000000 ) ;
#12318 = PRODUCT_DEFINITION_FORMATION_WITH_SPECIFIED_SOURCE ( 'ANY', '', #13924, .NOT_KNOWN. ) ;
#12319 = VERTEX_POINT ( 'NONE', #22609 ) ;
#12320 = VECTOR ( 'NONE', #5779, 1000.000000000000000 ) ;
#12321 = DIRECTION ( 'NONE',  ( -0.000000000000000000, -0.000000000000000000, -1.000000000000000000 ) ) ;
#12322 = EDGE_CURVE ( 'NONE', #22129, #13339, #3937, .T. ) ;
#12323 = ADVANCED_FACE ( 'NONE', ( #2233 ), #20417, .F. ) ;
#12324 = FACE_OUTER_BOUND ( 'NONE', #9815, .T. ) ;
#12325 = CARTESIAN_POINT ( 'NONE',  ( 23.00000000000000000, 10.59264252385243665, -4.936618945406485714 ) ) ;
#12326 = SURFACE_STYLE_USAGE ( .BOTH. , #6722 ) ;
#12327 = CIRCLE ( 'NONE', #1821, 5.099999999999996980 ) ;
#12328 = MECHANICAL_DESIGN_GEOMETRIC_PRESENTATION_REPRESENTATION (  '', ( #15439 ), #19755 ) ;
#12329 = DIRECTION ( 'NONE',  ( 1.000000000000000000, 0.000000000000000000, 0.000000000000000000 ) ) ;
#12330 = EDGE_LOOP ( 'NONE', ( #17115, #308, #682, #7453 ) ) ;
#12331 = CARTESIAN_POINT ( 'NONE',  ( -14.67187117805616481, 3.178673068337430241, 8.975236025575924259 ) ) ;
#12332 = ORIENTED_EDGE ( 'NONE', *, *, #18094, .F. ) ;
#12333 = DIRECTION ( 'NONE',  ( 1.000000000000000000, 0.000000000000000000, 0.000000000000000000 ) ) ;
#12334 = EDGE_LOOP ( 'NONE', ( #8705, #4730, #18980, #1051, #2603, #19132 ) ) ;
#12335 = CARTESIAN_POINT ( 'NONE',  ( -2.682529543900285862, 8.255977015246234174, 5.233165578109188587 ) ) ;
#12336 = CONICAL_SURFACE ( 'NONE', #4560, 5.000000000000007994, 0.9599310885968855844 ) ;
#12337 = VERTEX_POINT ( 'NONE', #2112 ) ;
#12338 = DIRECTION ( 'NONE',  ( 0.000000000000000000, -1.000000000000000000, 0.000000000000000000 ) ) ;
#12339 = DIRECTION ( 'NONE',  ( -0.000000000000000000, -0.000000000000000000, -1.000000000000000000 ) ) ;
#12340 = DIRECTION ( 'NONE',  ( -1.000000000000000000, 0.000000000000000000, 0.000000000000000000 ) ) ;
#12341 = CARTESIAN_POINT ( 'NONE',  ( -6.153822176767817416E-13, 9.500000000000000000, 3.706742014460231882 ) ) ;
#12342 = CARTESIAN_POINT ( 'NONE',  ( -23.90000000000000213, -29.49999999999999645, 0.000000000000000000 ) ) ;
#12343 = AXIS2_PLACEMENT_3D ( 'NONE', #20787, #2351, #2115 ) ;
#12344 = CARTESIAN_POINT ( 'NONE',  ( 9.499999999999790390, 3.086737114213260025, -7.306742014460234635 ) ) ;
#12345 = ORIENTED_EDGE ( 'NONE', *, *, #19330, .F. ) ;
#12346 = ORIENTED_EDGE ( 'NONE', *, *, #21639, .T. ) ;
#12347 = B_SPLINE_CURVE_WITH_KNOTS ( 'NONE', 3,
 ( #16061, #4988, #17796, #10558 ),
 .UNSPECIFIED., .F., .F.,
 ( 4, 4 ),
 ( 0.1802218513154718038, 1.000000000000000000 ),
 .UNSPECIFIED. ) ;
#12348 = EDGE_CURVE ( 'NONE', #11886, #2809, #17657, .T. ) ;
#12349 = ORIENTED_EDGE ( 'NONE', *, *, #22139, .F. ) ;
#12350 = CARTESIAN_POINT ( 'NONE',  ( 0.000000000000000000, 1.680940823232891723E-15, -13.72592346138681130 ) ) ;
#12351 = ADVANCED_FACE ( 'NONE', ( #21032 ), #13465, .T. ) ;
#12352 = ORIENTED_EDGE ( 'NONE', *, *, #5933, .T. ) ;
#12353 = CARTESIAN_POINT ( 'NONE',  ( 82.14750088563508257, -5.000000000000009770, 0.000000000000000000 ) ) ;
#12354 = PRODUCT_DEFINITION_SHAPE ( 'NONE', 'NONE',  #24099 ) ;
#12355 = DIRECTION ( 'NONE',  ( 0.000000000000000000, 0.000000000000000000, 1.000000000000000000 ) ) ;
#12356 = CARTESIAN_POINT ( 'NONE',  ( 69.05659179472598908, 7.420530141404717394E-15, 0.000000000000000000 ) ) ;
#12357 = CARTESIAN_POINT ( 'NONE',  ( 0.000000000000000000, 0.000000000000000000, -27.00000000000000000 ) ) ;
#12358 = ORIENTED_EDGE ( 'NONE', *, *, #18530, .T. ) ;
#12359 = DIRECTION ( 'NONE',  ( 0.000000000000000000, 0.000000000000000000, -1.000000000000000000 ) ) ;
#12360 = CARTESIAN_POINT ( 'NONE',  ( 90.00000000000000000, 0.000000000000000000, 0.000000000000000000 ) ) ;
#12361 = CARTESIAN_POINT ( 'NONE',  ( -42.00000000000000000, 4.000000000000000888, 10.49999999999999822 ) ) ;
#12362 = ORIENTED_EDGE ( 'NONE', *, *, #5933, .F. ) ;
#12363 = FACE_OUTER_BOUND ( 'NONE', #12411, .T. ) ;
#12364 = EDGE_CURVE ( 'NONE', #5671, #22129, #20781, .T. ) ;
#12365 = ORIENTED_EDGE ( 'NONE', *, *, #10596, .F. ) ;
#12366 = VERTEX_POINT ( 'NONE', #20561 ) ;
#12367 = EDGE_CURVE ( 'NONE', #4711, #13276, #19632, .T. ) ;
#12368 = VERTEX_POINT ( 'NONE', #7713 ) ;
#12369 = LINE ( 'NONE', #10421, #5329 ) ;
#12370 = DIRECTION ( 'NONE',  ( 0.000000000000000000, 0.000000000000000000, 1.000000000000000000 ) ) ;
#12371 = EDGE_CURVE ( 'NONE', #16325, #15649, #21558, .T. ) ;
#12372 = DIRECTION ( 'NONE',  ( -0.000000000000000000, -0.000000000000000000, -1.000000000000000000 ) ) ;
#12373 = VERTEX_POINT ( 'NONE', #20668 ) ;
#12374 = CARTESIAN_POINT ( 'NONE',  ( -17.19784311473119587, -8.411123426659422364, 4.422670359120423278 ) ) ;
#12375 = ADVANCED_FACE ( 'NONE', ( #18714 ), #19202, .T. ) ;
#12376 = DIRECTION ( 'NONE',  ( 0.000000000000000000, 0.000000000000000000, 1.000000000000000000 ) ) ;
#12377 = EDGE_LOOP ( 'NONE', ( #3849, #7850, #19692, #10495 ) ) ;
#12378 = CARTESIAN_POINT ( 'NONE',  ( -2.935661446561384391, -9.035036904804158553, -8.606742014460234458 ) ) ;
#12379 = CARTESIAN_POINT ( 'NONE',  ( -5.871322893123449127, -8.081182679344781405, 7.359589141758142716 ) ) ;
#12380 = CARTESIAN_POINT ( 'NONE',  ( -9.499999999999790390, -3.086737114213257804, 4.306742014460233747 ) ) ;
#12381 = ORIENTED_EDGE ( 'NONE', *, *, #684, .F. ) ;
#12382 = FACE_OUTER_BOUND ( 'NONE', #11354, .T. ) ;
#12383 = DIRECTION ( 'NONE',  ( 1.000000000000000000, 0.000000000000000000, 0.000000000000000000 ) ) ;
#12384 = AXIS2_PLACEMENT_3D ( 'NONE', #17914, #14119, #21580 ) ;
#12385 = CARTESIAN_POINT ( 'NONE',  ( -14.67173559926287396, -3.179195828807837909, 8.975010320294696697 ) ) ;
#12386 = DIRECTION ( 'NONE',  ( 0.000000000000000000, 0.000000000000000000, 1.000000000000000000 ) ) ;
#12387 = FACE_OUTER_BOUND ( 'NONE', #13016, .T. ) ;
#12388 = ORIENTED_EDGE ( 'NONE', *, *, #6236, .F. ) ;
#12389 = DIRECTION ( 'NONE',  ( -1.000000000000000000, 0.000000000000000000, 0.000000000000000000 ) ) ;
#12390 = EDGE_LOOP ( 'NONE', ( #5977, #11360, #5768, #464 ) ) ;
#12391 = CARTESIAN_POINT ( 'NONE',  ( -7.022953521755574080, 5.102474405759713783, -11.43316557810918965 ) ) ;
#12392 = CARTESIAN_POINT ( 'NONE',  ( 5.365059087799946447, -7.384370330706356178, 4.333165578109189120 ) ) ;
#12393 = EDGE_CURVE ( 'NONE', #5011, #22408, #15407, .T. ) ;
#12394 = DIRECTION ( 'NONE',  ( 0.000000000000000000, 0.000000000000000000, 1.000000000000000000 ) ) ;
#12395 = CARTESIAN_POINT ( 'NONE',  ( 0.000000000000000000, 0.000000000000000000, 12.50000000000000000 ) ) ;
#12396 = ORIENTED_EDGE ( 'NONE', *, *, #20182, .F. ) ;
#12397 = EDGE_LOOP ( 'NONE', ( #918, #23629, #22857 ) ) ;
#12398 = EDGE_CURVE ( 'NONE', #9485, #3124, #4082, .T. ) ;
#12399 = CARTESIAN_POINT ( 'NONE',  ( 74.57977184163763695, 5.000000000000015987, 0.000000000000000000 ) ) ;
#12400 = CARTESIAN_POINT ( 'NONE',  ( 9.500000000000000000, 6.470877716354879437E-13, -4.059589141758143782 ) ) ;
#12401 = AXIS2_PLACEMENT_3D ( 'NONE', #7279, #20825, #5705 ) ;
#12402 = AXIS2_PLACEMENT_3D ( 'NONE', #18831, #9543, #3714 ) ;
#12403 = AXIS2_PLACEMENT_3D ( 'NONE', #9165, #16362, #16491 ) ;
#12404 = CARTESIAN_POINT ( 'NONE',  ( 2.979900905946554435, 8.492461647028314076, 99.39919329559242556 ) ) ;
#12405 = CARTESIAN_POINT ( 'NONE',  ( -23.85000000000000497, 15.03999999999999915, -25.00000000000000000 ) ) ;
#12406 = CARTESIAN_POINT ( 'NONE',  ( 33.99999999999998579, 4.999999999999985789, 11.00000000000000000 ) ) ;
#12407 = LINE ( 'NONE', #6456, #17248 ) ;
#12408 = CARTESIAN_POINT ( 'NONE',  ( -36.00000000000000711, -51.00000000000000711, 0.5000000000000004441 ) ) ;
#12409 = ORIENTED_EDGE ( 'NONE', *, *, #74, .T. ) ;
#12410 = LINE ( 'NONE', #10914, #23078 ) ;
#12411 = EDGE_LOOP ( 'NONE', ( #6855, #22451, #7585, #18630 ) ) ;
#12412 = CARTESIAN_POINT ( 'NONE',  ( 0.000000000000000000, 45.00000000000000000, -27.00000000000000000 ) ) ;
#12413 = PLANE ( 'NONE',  #23905 ) ;
#12414 = CARTESIAN_POINT ( 'NONE',  ( 16.99687406587156957, 7.923972684219727114, 5.245599057861377368 ) ) ;
#12415 = FACE_OUTER_BOUND ( 'NONE', #14755, .T. ) ;
#12416 = VERTEX_POINT ( 'NONE', #669 ) ;
#12417 = CARTESIAN_POINT ( 'NONE',  ( 41.50000000000000000, 28.80990663662250739, 0.000000000000000000 ) ) ;
#12418 = EDGE_LOOP ( 'NONE', ( #13591, #19070, #7374, #13519, #4247 ) ) ;
#12419 = ORIENTED_EDGE ( 'NONE', *, *, #21264, .T. ) ;
#12420 = CARTESIAN_POINT ( 'NONE',  ( -7.685661446561619314, -5.583959896779019161, 3.259589141758143516 ) ) ;
#12421 = CARTESIAN_POINT ( 'NONE',  ( 9.500000000000000000, 6.470877716354879437E-13, 7.206742014460234103 ) ) ;
#12422 = ORIENTED_EDGE ( 'NONE', *, *, #1743, .T. ) ;
#12423 =( NAMED_UNIT ( * ) PLANE_ANGLE_UNIT ( ) SI_UNIT ( $, .RADIAN. ) );
#12424 = DIRECTION ( 'NONE',  ( 0.000000000000000000, 0.000000000000000000, 1.000000000000000000 ) ) ;
#12425 = CARTESIAN_POINT ( 'NONE',  ( 3.890962118697714531E-15, 15.50000000000000000, 19.70000000000000284 ) ) ;
#12426 = EDGE_CURVE ( 'NONE', #17472, #1813, #540, .T. ) ;
#12427 = CARTESIAN_POINT ( 'NONE',  ( 68.76159002345582394, 7.562528597612068045E-15, 0.000000000000000000 ) ) ;
#12428 = CYLINDRICAL_SURFACE ( 'NONE', #10350, 11.68650000001168721 ) ;
#12429 = EDGE_CURVE ( 'NONE', #3651, #3029, #14917, .T. ) ;
#12430 = FACE_OUTER_BOUND ( 'NONE', #3746, .T. ) ;
#12431 = ORIENTED_EDGE ( 'NONE', *, *, #23666, .F. ) ;
#12432 = DIRECTION ( 'NONE',  ( 0.000000000000000000, 0.000000000000000000, 1.000000000000000000 ) ) ;
#12433 = CARTESIAN_POINT ( 'NONE',  ( 60.32931906745326245, -9.244463733058732095E-30, 5.000000000000007994 ) ) ;
#12434 = DIRECTION ( 'NONE',  ( 0.000000000000000000, -1.000000000000000000, 0.000000000000000000 ) ) ;
#12435 = CARTESIAN_POINT ( 'NONE',  ( 0.000000000000000000, 0.000000000000000000, -12.00000000000000000 ) ) ;
#12436 = CARTESIAN_POINT ( 'NONE',  ( 41.00000000000000000, -6.000000000000015099, 11.00000000000000000 ) ) ;
#12437 = ORIENTED_EDGE ( 'NONE', *, *, #19214, .T. ) ;
#12438 = CARTESIAN_POINT ( 'NONE',  ( 74.00000000000001421, 7.491529369508391930E-15, 0.000000000000000000 ) ) ;
#12439 = ORIENTED_EDGE ( 'NONE', *, *, #10861, .F. ) ;
#12440 = EDGE_CURVE ( 'NONE', #17969, #1880, #6147, .T. ) ;
#12441 = CARTESIAN_POINT ( 'NONE',  ( 9.500000000000000000, 6.470877716354879437E-13, -6.059589141758143782 ) ) ;
#12442 = ORIENTED_EDGE ( 'NONE', *, *, #15188, .F. ) ;
#12443 = VECTOR ( 'NONE', #23392, 1000.000000000000000 ) ;
#12444 = CARTESIAN_POINT ( 'NONE',  ( 5.365059087799947335, -7.384370330706356178, 4.333165578109189120 ) ) ;
#12445 = DIRECTION ( 'NONE',  ( 0.000000000000000000, -1.000000000000000000, 0.000000000000000000 ) ) ;
#12446 = ORIENTED_EDGE ( 'NONE', *, *, #23067, .F. ) ;
#12447 = CARTESIAN_POINT ( 'NONE',  ( 8.199992213793557028, -2.961991314798682939, -12.49999999999999645 ) ) ;
#12448 = EDGE_CURVE ( 'NONE', #21069, #4705, #189, .T. ) ;
#12449 = LINE ( 'NONE', #19913, #14946 ) ;
#12450 = CARTESIAN_POINT ( 'NONE',  ( -5.871322893123449127, -8.081182679344781405, -3.359589141758143160 ) ) ;
#12451 = DIRECTION ( 'NONE',  ( -0.000000000000000000, -0.000000000000000000, -1.000000000000000000 ) ) ;
#12452 = ADVANCED_FACE ( 'NONE', ( #22511 ), #3949, .T. ) ;
#12453 = DIRECTION ( 'NONE',  ( -0.000000000000000000, -0.000000000000000000, -1.000000000000000000 ) ) ;
#12454 = EDGE_CURVE ( 'NONE', #9276, #22027, #21582, .T. ) ;
#12455 = EDGE_CURVE ( 'NONE', #16852, #2012, #22877, .T. ) ;
#12456 = FACE_OUTER_BOUND ( 'NONE', #20807, .T. ) ;
#12457 = CARTESIAN_POINT ( 'NONE',  ( 28.27483331787888332, -41.23752903419610050, -27.00000000000000000 ) ) ;
#12458 = CARTESIAN_POINT ( 'NONE',  ( 5.871322893123449127, 8.081182679344781405, -5.506742014460233925 ) ) ;
#12459 = ORIENTED_EDGE ( 'NONE', *, *, #317, .T. ) ;
#12460 = EDGE_LOOP ( 'NONE', ( #20153, #13978, #23924 ) ) ;
#12461 = DIRECTION ( 'NONE',  ( 1.000000000000000000, 0.000000000000000000, 0.000000000000000000 ) ) ;
#12462 = AXIS2_PLACEMENT_3D ( 'NONE', #12197, #18073, #6723 ) ;
#12463 = LINE ( 'NONE', #19817, #9257 ) ;
#12464 = ORIENTED_EDGE ( 'NONE', *, *, #4858, .T. ) ;
#12465 = CARTESIAN_POINT ( 'NONE',  ( -29.00000000000000000, 29.49999999999999645, 11.00000000000000000 ) ) ;
#12466 = ADVANCED_FACE ( 'NONE', ( #9663 ), #17113, .T. ) ;
#12467 = DIRECTION ( 'NONE',  ( 1.000000000000000000, 0.000000000000000000, 0.000000000000000000 ) ) ;
#12468 = VERTEX_POINT ( 'NONE', #2356 ) ;
#12469 = DIRECTION ( 'NONE',  ( -0.000000000000000000, -0.000000000000000000, 1.000000000000000000 ) ) ;
#12470 = DIRECTION ( 'NONE',  ( -0.000000000000000000, -1.000000000000000000, -0.000000000000000000 ) ) ;
#12471 = DIRECTION ( 'NONE',  ( -1.000000000000000000, -0.000000000000000000, 0.000000000000000000 ) ) ;
#12472 = CARTESIAN_POINT ( 'NONE',  ( -20.85000000000000497, -15.03999999999999737, 0.000000000000000000 ) ) ;
#12473 = VECTOR ( 'NONE', #10980, 999.9999999999998863 ) ;
#12474 = CIRCLE ( 'NONE', #1956, 5.000000000000000888 ) ;
#12475 = ORIENTED_EDGE ( 'NONE', *, *, #9325, .F. ) ;
#12476 = EDGE_CURVE ( 'NONE', #15840, #666, #18845, .T. ) ;
#12477 = ORIENTED_EDGE ( 'NONE', *, *, #24078, .F. ) ;
#12478 = ORIENTED_EDGE ( 'NONE', *, *, #22469, .F. ) ;
#12479 = ORIENTED_EDGE ( 'NONE', *, *, #2401, .T. ) ;
#12480 = CARTESIAN_POINT ( 'NONE',  ( 66.14750088563508257, 7.420530141404717394E-15, 0.000000000000000000 ) ) ;
#12481 = DIRECTION ( 'NONE',  ( -1.000000000000000000, -0.000000000000000000, -0.000000000000000000 ) ) ;
#12482 = CYLINDRICAL_SURFACE ( 'NONE', #9447, 4.999999999999997335 ) ;
#12483 = ORIENTED_EDGE ( 'NONE', *, *, #16306, .T. ) ;
#12484 = DIRECTION ( 'NONE',  ( 1.000000000000000000, 0.000000000000000000, 0.000000000000000000 ) ) ;
#12485 = DIRECTION ( 'NONE',  ( 0.000000000000000000, 1.000000000000000000, 0.000000000000000000 ) ) ;
#12486 = VERTEX_POINT ( 'NONE', #23476 ) ;
#12487 = CARTESIAN_POINT ( 'NONE',  ( 0.000000000000000000, 45.00000000000000000, 23.99999999999999645 ) ) ;
#12488 = DIRECTION ( 'NONE',  ( 0.000000000000000000, -0.000000000000000000, -1.000000000000000000 ) ) ;
#12489 = FACE_OUTER_BOUND ( 'NONE', #5278, .T. ) ;
#12490 = EDGE_LOOP ( 'NONE', ( #1073, #255, #10618, #13821 ) ) ;
#12491 = DIRECTION ( 'NONE',  ( 1.000000000000000000, 0.000000000000000000, -0.000000000000000000 ) ) ;
#12492 = CARTESIAN_POINT ( 'NONE',  ( 0.000000000000000000, 45.00000000000000000, 23.99999999999999645 ) ) ;
#12493 = CARTESIAN_POINT ( 'NONE',  ( 60.03431729618309021, -5.000000000000000000, 6.123233995736775157E-16 ) ) ;
#12494 = EDGE_CURVE ( 'NONE', #5306, #5307, #6524, .T. ) ;
#12495 = CARTESIAN_POINT ( 'NONE',  ( 23.85000000000000142, -15.03999999999999737, 0.000000000000000000 ) ) ;
#12496 = CARTESIAN_POINT ( 'NONE',  ( 5.365059087799946447, -7.384370330706356178, 12.33316557810918646 ) ) ;
#12497 = ORIENTED_EDGE ( 'NONE', *, *, #3886, .F. ) ;
#12498 = EDGE_CURVE ( 'NONE', #11723, #8481, #12218, .T. ) ;
#12499 = DIRECTION ( 'NONE',  ( 0.000000000000000000, 0.000000000000000000, 1.000000000000000000 ) ) ;
#12500 = AXIS2_PLACEMENT_3D ( 'NONE', #8422, #10374, #21613 ) ;
#12501 = ORIENTED_EDGE ( 'NONE', *, *, #22034, .F. ) ;
#12502 = CARTESIAN_POINT ( 'NONE',  ( -9.378401895172221003, -4.713374146359802882E-16, -12.12159810482778788 ) ) ;
#12503 = CARTESIAN_POINT ( 'NONE',  ( -7.685661446561619314, -5.583959896779019161, -7.259589141758143960 ) ) ;
#12504 = AXIS2_PLACEMENT_3D ( 'NONE', #11897, #7994, #13370 ) ;
#12505 = FACE_OUTER_BOUND ( 'NONE', #8096, .T. ) ;
#12506 = DIRECTION ( 'NONE',  ( 0.4999999999999998890, 0.8660254037844385966, 0.000000000000000000 ) ) ;
#12507 = CARTESIAN_POINT ( 'NONE',  ( 0.000000000000000000, -15.23000000000000220, 27.00000000000000000 ) ) ;
#12508 = DIRECTION ( 'NONE',  ( 0.000000000000000000, -1.000000000000000000, 0.000000000000000000 ) ) ;
#12509 = CARTESIAN_POINT ( 'NONE',  ( -19.84999999999999787, 16.67999999999985405, 14.50000000000000000 ) ) ;
#12510 = EDGE_CURVE ( 'NONE', #4194, #13484, #9466, .T. ) ;
#12511 = VERTEX_POINT ( 'NONE', #19573 ) ;
#12512 = LINE ( 'NONE', #20227, #14487 ) ;
#12513 = ORIENTED_EDGE ( 'NONE', *, *, #11115, .T. ) ;
#12514 = DIRECTION ( 'NONE',  ( 0.000000000000000000, 0.5000000000000011102, 0.8660254037844380415 ) ) ;
#12515 = PLANE ( 'NONE',  #2861 ) ;
#12516 = CARTESIAN_POINT ( 'NONE',  ( 14.51962751333974389, 3.765689428759029234, 8.721787840009197268 ) ) ;
#12517 = COLOUR_RGB ( '',0.7921568627450980005, 0.8196078431372548767, 0.9333333333333333481 ) ;
#12518 = DIRECTION ( 'NONE',  ( -1.000000000000000000, 0.000000000000000000, -0.000000000000000000 ) ) ;
#12519 = EDGE_CURVE ( 'NONE', #11467, #20567, #4437, .T. ) ;
#12520 = ORIENTED_EDGE ( 'NONE', *, *, #4394, .T. ) ;
#12521 = CIRCLE ( 'NONE', #2006, 1.499999999999994449 ) ;
#12522 = TOROIDAL_SURFACE ( 'NONE', #14855, 12.73082370883259706, 1.500000000000000000 ) ;
#12523 = DIRECTION ( 'NONE',  ( 0.000000000000000000, -1.000000000000000000, 0.000000000000000000 ) ) ;
#12524 = VERTEX_POINT ( 'NONE', #19822 ) ;
#12525 = EDGE_CURVE ( 'NONE', #145, #19949, #2616, .T. ) ;
#12526 = ORIENTED_EDGE ( 'NONE', *, *, #5918, .F. ) ;
#12527 = CARTESIAN_POINT ( 'NONE',  ( 5.871322893124553133, -8.081182679343980269, 7.759589141758143072 ) ) ;
#12528 = CARTESIAN_POINT ( 'NONE',  ( -7.685661446562381371, 5.583959896777970222, 6.006742014460233037 ) ) ;
#12529 = CARTESIAN_POINT ( 'NONE',  ( 40.00000000000000000, -29.50000000000000000, 27.00000000000000000 ) ) ;
#12530 = ORIENTED_EDGE ( 'NONE', *, *, #6889, .F. ) ;
#12531 = VERTEX_POINT ( 'NONE', #17737 ) ;
#12532 = FACE_OUTER_BOUND ( 'NONE', #13810, .T. ) ;
#12533 = CARTESIAN_POINT ( 'NONE',  ( 73.12522638709218370, 6.123233995736675563E-16, -5.000000000000007994 ) ) ;
#12534 = DIRECTION ( 'NONE',  ( -1.000000000000000000, 0.000000000000000000, 0.000000000000000000 ) ) ;
#12535 = DIRECTION ( 'NONE',  ( -1.000000000000000000, -1.224606353822377258E-16, -0.000000000000000000 ) ) ;
#12536 = AXIS2_PLACEMENT_3D ( 'NONE', #18870, #13006, #2153 ) ;
#12537 = CIRCLE ( 'NONE', #13714, 1.500000000000000000 ) ;
#12538 = CARTESIAN_POINT ( 'NONE',  ( 0.000000000000000000, -7.033831428820292331, 16.43291941292170577 ) ) ;
#12539 = CIRCLE ( 'NONE', #21911, 5.000000000000007994 ) ;
#12540 = CIRCLE ( 'NONE', #3986, 8.000000000000003553 ) ;
#12541 = AXIS2_PLACEMENT_3D ( 'NONE', #15148, #13332, #18357 ) ;
#12542 = PRODUCT_DEFINITION ( 'UNKNOWN', '', #2597, #590 ) ;
#12543 = AXIS2_PLACEMENT_3D ( 'NONE', #3813, #7691, #1966 ) ;
#12544 = CARTESIAN_POINT ( 'NONE',  ( 7.685661446561619314, 5.583959896779020049, 10.25958914175814485 ) ) ;
#12545 = DIRECTION ( 'NONE',  ( 1.000000000000000000, 2.600433232233976523E-16, -0.000000000000000000 ) ) ;
#12546 = CARTESIAN_POINT ( 'NONE',  ( 8.932474687540457481, -3.867868693691433268, -11.92830913002139503 ) ) ;
#12547 = DIRECTION ( 'NONE',  ( -1.000000000000000000, -1.224606353822377258E-16, -0.000000000000000000 ) ) ;
#12548 = EDGE_CURVE ( 'NONE', #13405, #16852, #21405, .T. ) ;
#12549 = EDGE_CURVE ( 'NONE', #22890, #16185, #19338, .T. ) ;
#12550 = CARTESIAN_POINT ( 'NONE',  ( 5.365059087798938364, 7.384370330707087149, -8.933165578109186100 ) ) ;
#12551 = CARTESIAN_POINT ( 'NONE',  ( 0.000000000000000000, 0.000000000000000000, 105.0000000000000000 ) ) ;
#12552 = ORIENTED_EDGE ( 'NONE', *, *, #3348, .F. ) ;
#12553 = CARTESIAN_POINT ( 'NONE',  ( -6.822232771736904647E-13, 9.988891130263535700, -6.559589141758143782 ) ) ;
#12554 = ORIENTED_EDGE ( 'NONE', *, *, #22501, .T. ) ;
#12555 = CIRCLE ( 'NONE', #15279, 5.000000000000007994 ) ;
#12556 = DIRECTION ( 'NONE',  ( -0.000000000000000000, -0.000000000000000000, -1.000000000000000000 ) ) ;
#12557 = AXIS2_PLACEMENT_3D ( 'NONE', #15353, #140, #14866 ) ;
#12558 = CIRCLE ( 'NONE', #15680, 2.024999999999999911 ) ;
#12559 = CARTESIAN_POINT ( 'NONE',  ( 74.00000000000001421, -4.172000000000000597, 5.616230220889771312E-16 ) ) ;
#12560 = CIRCLE ( 'NONE', #13346, 17.87500000001787726 ) ;
#12561 = VERTEX_POINT ( 'NONE', #3092 ) ;
#12562 = CARTESIAN_POINT ( 'NONE',  ( -2.024999999999999911, -45.00000000000000000, 0.000000000000000000 ) ) ;
#12563 = CARTESIAN_POINT ( 'NONE',  ( 69.05659179472598908, 7.420530141404717394E-15, 0.000000000000000000 ) ) ;
#12564 = DIRECTION ( 'NONE',  ( -1.000000000000000000, -0.000000000000000000, 0.000000000000000000 ) ) ;
#12565 = CIRCLE ( 'NONE', #15686, 6.050000000006051870 ) ;
#12566 = DIRECTION ( 'NONE',  ( -1.000000000000000000, -1.224606353822377258E-16, -0.000000000000000000 ) ) ;
#12567 = CIRCLE ( 'NONE', #906, 14.42592346043842255 ) ;
#12568 = ORIENTED_EDGE ( 'NONE', *, *, #4568, .F. ) ;
#12569 = FACE_OUTER_BOUND ( 'NONE', #3777, .T. ) ;
#12570 = DIRECTION ( 'NONE',  ( 0.000000000000000000, 0.000000000000000000, 1.000000000000000000 ) ) ;
#12571 = EDGE_CURVE ( 'NONE', #6030, #15685, #11806, .T. ) ;
#12572 = CARTESIAN_POINT ( 'NONE',  ( 2.935661446562616295, -9.035036904803758873, -4.806742014460232859 ) ) ;
#12573 = EDGE_LOOP ( 'NONE', ( #15136, #22128, #19463, #7915 ) ) ;
#12574 = ORIENTED_EDGE ( 'NONE', *, *, #15980, .F. ) ;
#12575 = CARTESIAN_POINT ( 'NONE',  ( 23.00000000000000000, -6.393861490227931377, 9.782270569456429143 ) ) ;
#12576 = DIRECTION ( 'NONE',  ( 0.7052211081716914798, -0.7089874389501492624, 0.000000000000000000 ) ) ;
#12577 = VECTOR ( 'NONE', #23389, 1000.000000000000000 ) ;
#12578 = CARTESIAN_POINT ( 'NONE',  ( -30.68762588338048403, 45.64284848299540442, -1.500000000000000000 ) ) ;
#12579 = CIRCLE ( 'NONE', #14907, 3.500000000000003109 ) ;
#12580 = DIRECTION ( 'NONE',  ( 0.000000000000000000, 0.000000000000000000, 1.000000000000000000 ) ) ;
#12581 = VECTOR ( 'NONE', #12773, 1000.000000000000000 ) ;
#12582 = CIRCLE ( 'NONE', #18453, 5.000000000000007994 ) ;
#12583 = ADVANCED_FACE ( 'NONE', ( #13700 ), #4834, .T. ) ;
#12584 = ORIENTED_EDGE ( 'NONE', *, *, #9757, .F. ) ;
#12585 = ADVANCED_FACE ( 'NONE', ( #10024 ), #18450, .T. ) ;
#12586 = AXIS2_PLACEMENT_3D ( 'NONE', #4770, #8415, #16097 ) ;
#12587 = DIRECTION ( 'NONE',  ( 1.000000000000000000, 0.000000000000000000, 0.000000000000000000 ) ) ;
#12588 = CARTESIAN_POINT ( 'NONE',  ( 14.91530227160598798, -1.623290104782664445, 9.365835742197226921 ) ) ;
#12589 = ORIENTED_EDGE ( 'NONE', *, *, #11974, .F. ) ;
#12590 =( REPRESENTATION_RELATIONSHIP ('NONE','NONE', #21748, #15960 ) REPRESENTATION_RELATIONSHIP_WITH_TRANSFORMATION ( #18955 )SHAPE_REPRESENTATION_RELATIONSHIP( ) );
#12591 = DIRECTION ( 'NONE',  ( 0.000000000000000000, -1.000000000000000000, 0.000000000000000000 ) ) ;
#12592 = LINE ( 'NONE', #16019, #107 ) ;
#12593 = CARTESIAN_POINT ( 'NONE',  ( 40.23082370883257397, -27.62204025492844650, -1.500000000000000000 ) ) ;
#12594 = DIRECTION ( 'NONE',  ( 0.000000000000000000, -1.000000000000000000, 0.000000000000000000 ) ) ;
#12595 = VECTOR ( 'NONE', #5842, 1000.000000000000000 ) ;
#12596 = ORIENTED_EDGE ( 'NONE', *, *, #15911, .F. ) ;
#12597 = ORIENTED_EDGE ( 'NONE', *, *, #3886, .T. ) ;
#12598 = CIRCLE ( 'NONE', #14553, 5.000000000000007994 ) ;
#12599 = CIRCLE ( 'NONE', #17289, 9.000000000000000000 ) ;
#12600 = CIRCLE ( 'NONE', #15661, 1.999999999999994449 ) ;
#12601 = ORIENTED_EDGE ( 'NONE', *, *, #19302, .F. ) ;
#12603 = ORIENTED_EDGE ( 'NONE', *, *, #16032, .T. ) ;
#12602 = AXIS2_PLACEMENT_3D ( 'NONE', #21795, #10668, #18139 ) ;
#12604 = CARTESIAN_POINT ( 'NONE',  ( -31.74999999999995737, 0.000000000000000000, 0.000000000000000000 ) ) ;
#12605 = CARTESIAN_POINT ( 'NONE',  ( 0.000000000000000000, 15.23000000000000220, -27.00000000000000000 ) ) ;
#12606 = EDGE_CURVE ( 'NONE', #5444, #8401, #15640, .T. ) ;
#12607 = CARTESIAN_POINT ( 'NONE',  ( -34.00000000000000000, 5.999999999999999112, 12.00000000000000000 ) ) ;
#12608 = ORIENTED_EDGE ( 'NONE', *, *, #2845, .T. ) ;
#12609 = AXIS2_PLACEMENT_3D ( 'NONE', #7659, #15099, #5844 ) ;
#12610 = VERTEX_POINT ( 'NONE', #23108 ) ;
#12611 = CARTESIAN_POINT ( 'NONE',  ( 0.000000000000000000, 45.00000000000000000, -2.974999999999996092 ) ) ;
#12612 = VERTEX_POINT ( 'NONE', #8462 ) ;
#12613 = DIRECTION ( 'NONE',  ( -1.000000000000000000, 0.000000000000000000, 0.000000000000000000 ) ) ;
#12614 = FACE_OUTER_BOUND ( 'NONE', #16719, .T. ) ;
#12615 = FACE_OUTER_BOUND ( 'NONE', #19471, .T. ) ;
#12616 = EDGE_CURVE ( 'NONE', #20236, #18123, #22356, .T. ) ;
#12617 = DIRECTION ( 'NONE',  ( -1.000000000000000000, 0.000000000000000000, 0.000000000000000000 ) ) ;
#12618 = ADVANCED_FACE ( 'NONE', ( #19450 ), #2729, .T. ) ;
#12619 = CARTESIAN_POINT ( 'NONE',  ( -28.99999999999998579, -29.50000000000000711, -1.500000000000000000 ) ) ;
#12620 = DIRECTION ( 'NONE',  ( 0.000000000000000000, 0.000000000000000000, 1.000000000000000000 ) ) ;
#12621 = CIRCLE ( 'NONE', #5618, 5.000000000000007994 ) ;
#12622 = DIRECTION ( 'NONE',  ( 0.000000000000000000, 0.7557495743542551603, 0.6548607339452887643 ) ) ;
#12623 = VECTOR ( 'NONE', #20644, 1000.000000000000000 ) ;
#12624 = DIRECTION ( 'NONE',  ( -0.000000000000000000, -0.000000000000000000, -1.000000000000000000 ) ) ;
#12625 = CARTESIAN_POINT ( 'NONE',  ( 2.024999999999999911, 45.00000000000000000, -27.00000000000000000 ) ) ;
#12626 = AXIS2_PLACEMENT_3D ( 'NONE', #9067, #3355, #16519 ) ;
#12627 = ORIENTED_EDGE ( 'NONE', *, *, #22860, .F. ) ;
#12628 = CARTESIAN_POINT ( 'NONE',  ( -5.365059087798939252, -7.384370330707086261, 9.933165578109189653 ) ) ;
#12629 = ORIENTED_EDGE ( 'NONE', *, *, #3005, .F. ) ;
#12630 = AXIS2_PLACEMENT_3D ( 'NONE', #10464, #21713, #12039 ) ;
#12631 = LINE ( 'NONE', #1663, #17935 ) ;
#12632 = VERTEX_POINT ( 'NONE', #10283 ) ;
#12633 = ORIENTED_EDGE ( 'NONE', *, *, #24097, .T. ) ;
#12634 = CARTESIAN_POINT ( 'NONE',  ( 68.18181818181818699, 7.491529369508391930E-15, 0.000000000000000000 ) ) ;
#12635 = CARTESIAN_POINT ( 'NONE',  ( 5.871322893123449127, 8.081182679344781405, -4.359589141758143604 ) ) ;
#12636=STYLED_ITEM('',(#24141),#2432);
#12637 = VECTOR ( 'NONE', #20732, 1000.000000000000000 ) ;
#12638 = CYLINDRICAL_SURFACE ( 'NONE', #3270, 6.050000000006050982 ) ;
#12639 = DIRECTION ( 'NONE',  ( -0.000000000000000000, -0.000000000000000000, -1.000000000000000000 ) ) ;
#12640 = FACE_OUTER_BOUND ( 'NONE', #11543, .T. ) ;
#12641 = AXIS2_PLACEMENT_3D ( 'NONE', #4854, #6669, #19738 ) ;
#12642 = DIRECTION ( 'NONE',  ( -1.000000000000000000, -4.625929269271481378E-15, 0.000000000000000000 ) ) ;
#12643 = ORIENTED_EDGE ( 'NONE', *, *, #23866, .T. ) ;
#12644 = DIRECTION ( 'NONE',  ( -0.000000000000000000, -0.000000000000000000, 1.000000000000000000 ) ) ;
#12645 = VECTOR ( 'NONE', #4519, 1000.000000000000000 ) ;
#12646 = VERTEX_POINT ( 'NONE', #1039 ) ;
#12647 = CARTESIAN_POINT ( 'NONE',  ( 9.324366623732823450E-16, 6.000000000000000000, 77.99999999999998579 ) ) ;
#12648 = ADVANCED_FACE ( 'NONE', ( #15906 ), #23370, .T. ) ;
#12649 = CARTESIAN_POINT ( 'NONE',  ( -41.00000000000000000, -6.000000000000000888, 11.00000000000000000 ) ) ;
#12650 = DIRECTION ( 'NONE',  ( -5.501724186093582121E-16, 1.000000000000000000, -0.000000000000000000 ) ) ;
#12651 = CARTESIAN_POINT ( 'NONE',  ( 17.32141611691247718, 8.728455122802976973, 3.780491077225283103 ) ) ;
#12652 = VECTOR ( 'NONE', #14002, 1000.000000000000000 ) ;
#12653 = CARTESIAN_POINT ( 'NONE',  ( 0.000000000000000000, -45.00000000000000000, -3.000000000000000000 ) ) ;
#12654 = ORIENTED_EDGE ( 'NONE', *, *, #8113, .T. ) ;
#12655 = CARTESIAN_POINT ( 'NONE',  ( -31.74999999999995737, 0.000000000000000000, 0.000000000000000000 ) ) ;
#12656 = FACE_OUTER_BOUND ( 'NONE', #16081, .T. ) ;
#12657 = ORIENTED_EDGE ( 'NONE', *, *, #20814, .F. ) ;
#12658 = EDGE_LOOP ( 'NONE', ( #5262, #4761, #18727, #4469 ) ) ;
#12659 = CARTESIAN_POINT ( 'NONE',  ( 9.499999999999790390, 3.086737114213260025, 11.30674201446023019 ) ) ;
#12660 = CARTESIAN_POINT ( 'NONE',  ( 7.685661446562381371, -5.583959896777971110, 9.006742014460233037 ) ) ;
#12661 = CARTESIAN_POINT ( 'NONE',  ( -0.7000000000000005107, 0.000000000000000000, 4.000000000000000000 ) ) ;
#12662 = VERTEX_POINT ( 'NONE', #19706 ) ;
#12663 = VERTEX_POINT ( 'NONE', #10412 ) ;
#12664 = CARTESIAN_POINT ( 'NONE',  ( 23.00000000000000000, -7.033831428820288778, 16.43291941292170577 ) ) ;
#12665 = VECTOR ( 'NONE', #9477, 1000.000000000000000 ) ;
#12666 = DIRECTION ( 'NONE',  ( -1.000000000000000000, -0.000000000000000000, -0.000000000000000000 ) ) ;
#12667 = CARTESIAN_POINT ( 'NONE',  ( -7.685661446561619314, -5.583959896779019161, -4.406742014460233392 ) ) ;
#12668 = EDGE_CURVE ( 'NONE', #5490, #23000, #17865, .T. ) ;
#12669 = AXIS2_PLACEMENT_3D ( 'NONE', #3523, #23679, #10931 ) ;
#12670 = CONICAL_SURFACE ( 'NONE', #13066, 2.024999999999999911, 0.7853981633974222998 ) ;
#12671 = CONICAL_SURFACE ( 'NONE', #17733, 5.000000000000007994, 0.9599310885968855844 ) ;
#12672 = DIRECTION ( 'NONE',  ( -0.000000000000000000, -0.000000000000000000, 1.000000000000000000 ) ) ;
#12673 = CARTESIAN_POINT ( 'NONE',  ( 74.57977184163763695, 7.562528597612068045E-15, 0.000000000000000000 ) ) ;
#12674 = EDGE_CURVE ( 'NONE', #14048, #22424, #15721, .T. ) ;
#12675 = EDGE_CURVE ( 'NONE', #19252, #379, #11102, .T. ) ;
#12676 = EDGE_CURVE ( 'NONE', #13598, #11604, #21529, .T. ) ;
#12677 = CIRCLE ( 'NONE', #10407, 1.000000000000000888 ) ;
#12678 = CARTESIAN_POINT ( 'NONE',  ( 0.000000000000000000, 0.000000000000000000, 12.50000000000000000 ) ) ;
#12679 = CARTESIAN_POINT ( 'NONE',  ( -30.44534269664590553, -40.40463133211081015, 11.00000000000000000 ) ) ;
#12680 = CARTESIAN_POINT ( 'NONE',  ( 6.809999908187194197E-13, -9.988891130263535700, -11.55958914175814201 ) ) ;
#12681 = CIRCLE ( 'NONE', #12284, 5.000000000000007994 ) ;
#12682 = CARTESIAN_POINT ( 'NONE',  ( -34.10000000000000142, 29.50000000000000000, -27.00000000000000000 ) ) ;
#12683 = CARTESIAN_POINT ( 'NONE',  ( -2.682529543899159208, -8.255977015246598327, -8.033165578109189298 ) ) ;
#12684 = AXIS2_PLACEMENT_3D ( 'NONE', #23280, #14097, #1068 ) ;
#12685 = CARTESIAN_POINT ( 'NONE',  ( -14.94708199919714176, 1.300481340138139430, 9.416259293296523225 ) ) ;
#12686 = VECTOR ( 'NONE', #5323, 1000.000000000000000 ) ;
#12687 = VERTEX_POINT ( 'NONE', #16142 ) ;
#12688 = DIRECTION ( 'NONE',  ( -0.000000000000000000, -0.000000000000000000, 1.000000000000000000 ) ) ;
#12689 = VERTEX_POINT ( 'NONE', #3455 ) ;
#12690 = CARTESIAN_POINT ( 'NONE',  ( 21.13207267780287069, 38.32709852940855910, 11.00000000000000000 ) ) ;
#12691 = DIRECTION ( 'NONE',  ( -0.000000000000000000, -0.000000000000000000, -1.000000000000000000 ) ) ;
#12692 = ORIENTED_EDGE ( 'NONE', *, *, #4568, .T. ) ;
#12693 = CARTESIAN_POINT ( 'NONE',  ( 8.746907971560203165, -1.213523871515275410, -12.49999999999999289 ) ) ;
#12694 = FACE_BOUND ( 'NONE', #22841, .T. ) ;
#12695 = DIRECTION ( 'NONE',  ( -0.000000000000000000, -0.000000000000000000, -1.000000000000000000 ) ) ;
#12696 = DIRECTION ( 'NONE',  ( -1.000000000000000000, 0.000000000000000000, 0.000000000000000000 ) ) ;
#12697 = CIRCLE ( 'NONE', #248, 5.000000000000007994 ) ;
#12698 =( GEOMETRIC_REPRESENTATION_CONTEXT ( 3 ) GLOBAL_UNCERTAINTY_ASSIGNED_CONTEXT ( ( #13256 ) ) GLOBAL_UNIT_ASSIGNED_CONTEXT ( ( #21358, #2681, #4393 ) ) REPRESENTATION_CONTEXT ( 'NONE', 'WORKASPACE' ) );
#12699 = AXIS2_PLACEMENT_3D ( 'NONE', #8775, #12535, #7055 ) ;
#12700 = EDGE_LOOP ( 'NONE', ( #14644, #14705, #4340, #3635, #22722, #22886 ) ) ;
#12701 = CARTESIAN_POINT ( 'NONE',  ( 6.699999999999999289, 1.717680227207312385E-15, -14.02592346138681201 ) ) ;
#12702 = EDGE_CURVE ( 'NONE', #3850, #2350, #5208, .T. ) ;
#12703 = DIRECTION ( 'NONE',  ( -1.000000000000000000, -0.000000000000000000, -0.000000000000000000 ) ) ;
#12704 = EDGE_CURVE ( 'NONE', #19865, #15990, #7518, .T. ) ;
#12705 = CIRCLE ( 'NONE', #11914, 9.747164428915397139 ) ;
#12706 = CARTESIAN_POINT ( 'NONE',  ( -1.504652183083727168, 9.499999999999904077, -3.757996296007079184 ) ) ;
#12707 = ORIENTED_EDGE ( 'NONE', *, *, #2688, .T. ) ;
#12708 = ORIENTED_EDGE ( 'NONE', *, *, #14810, .T. ) ;
#12709 = CARTESIAN_POINT ( 'NONE',  ( -9.999999999999998224, 0.000000000000000000, 15.50000000000000000 ) ) ;
#12710 = CYLINDRICAL_SURFACE ( 'NONE', #3426, 10.99999999999999645 ) ;
#12711 = DIRECTION ( 'NONE',  ( 1.000000000000000000, 0.000000000000000000, 0.000000000000000000 ) ) ;
#12712 = VERTEX_POINT ( 'NONE', #16619 ) ;
#12713 = VECTOR ( 'NONE', #15131, 999.9999999999998863 ) ;
#12714 = DIRECTION ( 'NONE',  ( -1.000000000000000000, 0.000000000000000000, 0.000000000000000000 ) ) ;
#12715 = CARTESIAN_POINT ( 'NONE',  ( 15.00000000000000178, -0.3242076166095157475, 9.499999999999987566 ) ) ;
#12716 = AXIS2_PLACEMENT_3D ( 'NONE', #8207, #13487, #800 ) ;
#12717 = LINE ( 'NONE', #10413, #20786 ) ;
#12718 = ORIENTED_EDGE ( 'NONE', *, *, #4574, .F. ) ;
#12719 = DIRECTION ( 'NONE',  ( -1.000000000000000000, -1.224606353822377258E-16, -0.000000000000000000 ) ) ;
#12720 = DIRECTION ( 'NONE',  ( -1.000000000000000000, -1.224606353822377258E-16, -0.000000000000000000 ) ) ;
#12721 = FACE_OUTER_BOUND ( 'NONE', #19038, .T. ) ;
#12722 = AXIS2_PLACEMENT_3D ( 'NONE', #22089, #21833, #20004 ) ;
#12723 = DIRECTION ( 'NONE',  ( -1.000000000000000000, -0.000000000000000000, -0.000000000000000000 ) ) ;
#12724 = EDGE_LOOP ( 'NONE', ( #14180, #20532, #11702, #22237 ) ) ;
#12725 = AXIS2_PLACEMENT_3D ( 'NONE', #9300, #16744, #7588 ) ;
#12726 = EDGE_CURVE ( 'NONE', #3029, #13623, #9854, .T. ) ;
#12727 = ORIENTED_EDGE ( 'NONE', *, *, #3647, .T. ) ;
#12728 = ADVANCED_FACE ( 'NONE', ( #20400 ), #1268, .T. ) ;
#12729 = ORIENTED_EDGE ( 'NONE', *, *, #12476, .T. ) ;
#12730 = CARTESIAN_POINT ( 'NONE',  ( 9.000000000000000000, 0.000000000000000000, 0.9999999999999940048 ) ) ;
#12731 = ADVANCED_FACE ( 'NONE', ( #160 ), #6122, .F. ) ;
#12732 = AXIS2_PLACEMENT_3D ( 'NONE', #11845, #17714, #11964 ) ;
#12733 = CARTESIAN_POINT ( 'NONE',  ( -42.00000000000000000, 25.22443390181682688, -0.6213203435596427182 ) ) ;
#12734 = DIRECTION ( 'NONE',  ( 0.000000000000000000, 1.000000000000000000, 0.000000000000000000 ) ) ;
#12735 = ORIENTED_EDGE ( 'NONE', *, *, #14379, .F. ) ;
#12736 = EDGE_LOOP ( 'NONE', ( #14338, #21178, #17748, #8341 ) ) ;
#12737 = CARTESIAN_POINT ( 'NONE',  ( -23.89999999999999858, 29.50000000000000000, 27.00000000000000000 ) ) ;
#12738 = ORIENTED_EDGE ( 'NONE', *, *, #23696, .F. ) ;
#12739 = LINE ( 'NONE', #9194, #17047 ) ;
#12740 = DIRECTION ( 'NONE',  ( -0.000000000000000000, -0.000000000000000000, 1.000000000000000000 ) ) ;
#12741 = APPLICATION_CONTEXT ( 'automotive_design' ) ;
#12742 = CARTESIAN_POINT ( 'NONE',  ( 2.024999999999999911, 45.00000000000000000, -27.00000000000000000 ) ) ;
#12743 = DIRECTION ( 'NONE',  ( 0.000000000000000000, -1.000000000000000000, 0.000000000000000000 ) ) ;
#12744 = CARTESIAN_POINT ( 'NONE',  ( -30.68762588338048403, 45.64284848299540442, -3.000000000000000000 ) ) ;
#12745 = FACE_OUTER_BOUND ( 'NONE', #13462, .T. ) ;
#12746 = LINE ( 'NONE', #18611, #11507 ) ;
#12747 = EDGE_LOOP ( 'NONE', ( #5236, #2366, #7141, #10169, #9377, #12345 ) ) ;
#12748 = CARTESIAN_POINT ( 'NONE',  ( 7.022953521754877748, 5.102474405760673903, 10.83316557810919001 ) ) ;
#12749 = EDGE_CURVE ( 'NONE', #3260, #4159, #4042, .T. ) ;
#12750 = ORIENTED_EDGE ( 'NONE', *, *, #15555, .T. ) ;
#12751 = SHAPE_DEFINITION_REPRESENTATION ( #13270, #23456 ) ;
#12752 = CARTESIAN_POINT ( 'NONE',  ( 4.489900896931573904, 0.000000000000000000, 11.24716442891539359 ) ) ;
#12753 = ORIENTED_EDGE ( 'NONE', *, *, #12261, .T. ) ;
#12754 = ORIENTED_EDGE ( 'NONE', *, *, #15110, .F. ) ;
#12755 = ADVANCED_FACE ( 'NONE', ( #4052 ), #2472, .T. ) ;
#12756 = LINE ( 'NONE', #7273, #22406 ) ;
#12757 = CARTESIAN_POINT ( 'NONE',  ( 9.500000000000209610, -3.086737114211962396, -5.959589141758143249 ) ) ;
#12758 = EDGE_CURVE ( 'NONE', #13595, #17414, #7928, .T. ) ;
#12759 = AXIS2_PLACEMENT_3D ( 'NONE', #23239, #4685, #21511 ) ;
#12760 = DIRECTION ( 'NONE',  ( -0.5735764363510519326, 0.8191520442889876907, 1.003171929053519816E-16 ) ) ;
#12761 = FACE_OUTER_BOUND ( 'NONE', #9056, .T. ) ;
#12762 = DIRECTION ( 'NONE',  ( -1.000000000000000000, 0.000000000000000000, 0.000000000000000000 ) ) ;
#12763 = CARTESIAN_POINT ( 'NONE',  ( 9.999999999999998224, 1.224646799147353059E-15, 15.50000000000000000 ) ) ;
#12764 = EDGE_LOOP ( 'NONE', ( #22788, #631, #7744, #4614 ) ) ;
#12765 = VECTOR ( 'NONE', #19563, 1000.000000000000000 ) ;
#12766 = CARTESIAN_POINT ( 'NONE',  ( 6.809999908187194197E-13, -9.988891130263535700, -6.706742014460232326 ) ) ;
#12767 = ORIENTED_EDGE ( 'NONE', *, *, #7246, .T. ) ;
#12768 = ORIENTED_EDGE ( 'NONE', *, *, #4575, .T. ) ;
#12769 = DIRECTION ( 'NONE',  ( -0.000000000000000000, -0.000000000000000000, 1.000000000000000000 ) ) ;
#12770 = CARTESIAN_POINT ( 'NONE',  ( 0.000000000000000000, 0.000000000000000000, 0.4999999999999995559 ) ) ;
#12771 = DIRECTION ( 'NONE',  ( 1.000000000000000000, 0.000000000000000000, 0.000000000000000000 ) ) ;
#12772 = CARTESIAN_POINT ( 'NONE',  ( 5.000000000000000000, 5.258101095580061836E-15, 4.057500000000008100 ) ) ;
#12773 = DIRECTION ( 'NONE',  ( 0.000000000000000000, -1.000000000000000000, 0.000000000000000000 ) ) ;
#12774 = CARTESIAN_POINT ( 'NONE',  ( 7.685661446562381371, -5.583959896777971110, -11.00674201446023304 ) ) ;
#12775 = LINE ( 'NONE', #12889, #12096 ) ;
#12776 = ORIENTED_EDGE ( 'NONE', *, *, #19488, .F. ) ;
#12777 = EDGE_CURVE ( 'NONE', #5416, #7845, #22849, .T. ) ;
#12778 = VERTEX_POINT ( 'NONE', #9746 ) ;
#12779 = CARTESIAN_POINT ( 'NONE',  ( -6.822232771736903637E-13, 9.988891130263535700, 9.706742014460232326 ) ) ;
#12780 = CARTESIAN_POINT ( 'NONE',  ( 9.500000000000209610, -3.086737114211962396, 9.106742014460232681 ) ) ;
#12781 = ORIENTED_EDGE ( 'NONE', *, *, #22971, .F. ) ;
#12782 = CIRCLE ( 'NONE', #2270, 5.000000000000007994 ) ;
#12783 = ORIENTED_EDGE ( 'NONE', *, *, #4941, .T. ) ;
#12784 = AXIS2_PLACEMENT_3D ( 'NONE', #11212, #18329, #10969 ) ;
#12785 = DIRECTION ( 'NONE',  ( 0.000000000000000000, -1.000000000000000000, 0.000000000000000000 ) ) ;
#12786 = FACE_OUTER_BOUND ( 'NONE', #5106, .T. ) ;
#12787 = EDGE_CURVE ( 'NONE', #16231, #14736, #20800, .T. ) ;
#12788 = ADVANCED_FACE ( 'NONE', ( #4298 ), #7565, .T. ) ;
#12789 = DIRECTION ( 'NONE',  ( 0.000000000000000000, 0.000000000000000000, 1.000000000000000000 ) ) ;
#12790 = DIRECTION ( 'NONE',  ( 0.000000000000000000, 0.000000000000000000, 1.000000000000000000 ) ) ;
#12791 = DIRECTION ( 'NONE',  ( 1.000000000000000000, 1.224606353822377258E-16, 0.000000000000000000 ) ) ;
#12792 = ORIENTED_EDGE ( 'NONE', *, *, #14350, .F. ) ;
#12793 = CIRCLE ( 'NONE', #2280, 5.000000000000007994 ) ;
#12794 = CARTESIAN_POINT ( 'NONE',  ( 7.685661446561619314, 5.583959896779020049, -10.25958914175814485 ) ) ;
#12795 = CARTESIAN_POINT ( 'NONE',  ( 3.890962118697714531E-15, 15.50000000000000000, 16.70000000000000284 ) ) ;
#12796 = ORIENTED_EDGE ( 'NONE', *, *, #16620, .F. ) ;
#12797 = DIRECTION ( 'NONE',  ( -1.000000000000000000, 0.000000000000000000, 0.000000000000000000 ) ) ;
#12798 = CARTESIAN_POINT ( 'NONE',  ( 18.49999999999999645, -15.23000000000000043, 27.00000000000000000 ) ) ;
#12799 = CARTESIAN_POINT ( 'NONE',  ( -28.99999999999999645, 29.50000000000000000, -27.00000000000000000 ) ) ;
#12800 = CARTESIAN_POINT ( 'NONE',  ( 9.500000000000000000, 1.163414459189985485E-15, 12.50000000000000000 ) ) ;
#12801 = CARTESIAN_POINT ( 'NONE',  ( 23.00000000000000000, 3.378881074890460745, -11.18737882312118082 ) ) ;
#12802 = EDGE_CURVE ( 'NONE', #11149, #16191, #19257, .T. ) ;
#12803 = DIRECTION ( 'NONE',  ( 0.4828336235133043330, 0.8757121056631641531, -0.000000000000000000 ) ) ;
#12804 = EDGE_LOOP ( 'NONE', ( #19777, #15106, #14825, #3854 ) ) ;
#12805 = LINE ( 'NONE', #1941, #17326 ) ;
#12806 = ORIENTED_EDGE ( 'NONE', *, *, #12137, .T. ) ;
#12807 = EDGE_CURVE ( 'NONE', #6224, #4642, #16130, .T. ) ;
#12808 = DIRECTION ( 'NONE',  ( 0.000000000000000000, -1.000000000000000000, 0.000000000000000000 ) ) ;
#12809 = ORIENTED_EDGE ( 'NONE', *, *, #9088, .T. ) ;
#12810 = DIRECTION ( 'NONE',  ( -0.000000000000000000, -0.000000000000000000, -1.000000000000000000 ) ) ;
#12811 = DIRECTION ( 'NONE',  ( 0.000000000000000000, 0.000000000000000000, 1.000000000000000000 ) ) ;
#12812 = EDGE_CURVE ( 'NONE', #15518, #7322, #1346, .T. ) ;
#12813 = DIRECTION ( 'NONE',  ( -0.000000000000000000, -0.000000000000000000, 1.000000000000000000 ) ) ;
#12814 = ADVANCED_FACE ( 'NONE', ( #3807 ), #32, .T. ) ;
#12815 = SHAPE_REPRESENTATION ( 'Assembly Drive shaft gear', ( #2965, #16583, #18172 ), #1790 ) ;
#12816 = CARTESIAN_POINT ( 'NONE',  ( 5.378177448618336243, 1.359010689748310618E-15, -10.94716442891539465 ) ) ;
#12817 = CARTESIAN_POINT ( 'NONE',  ( -9.499999999999790390, -3.086737114213257804, -9.159589141758145203 ) ) ;
#12818 = ORIENTED_EDGE ( 'NONE', *, *, #18792, .F. ) ;
#12819 = ORIENTED_EDGE ( 'NONE', *, *, #3072, .T. ) ;
#12820 = DIRECTION ( 'NONE',  ( -0.000000000000000000, 0.000000000000000000, 1.000000000000000000 ) ) ;
#12821 = AXIS2_PLACEMENT_3D ( 'NONE', #5590, #16792, #458 ) ;
#12822 = FACE_OUTER_BOUND ( 'NONE', #6211, .T. ) ;
#12823 = SURFACE_STYLE_USAGE ( .BOTH. , #14664 ) ;
#12824 = ORIENTED_EDGE ( 'NONE', *, *, #6677, .T. ) ;
#12825 = ADVANCED_FACE ( 'NONE', ( #3921 ), #2495, .F. ) ;
#12826 = CARTESIAN_POINT ( 'NONE',  ( -31.74999999999995737, 6.123233995736767268E-16, -5.000000000000000888 ) ) ;
#12827 = DIRECTION ( 'NONE',  ( 1.000000000000000000, 0.000000000000000000, 0.000000000000000000 ) ) ;
#12828 = ORIENTED_EDGE ( 'NONE', *, *, #10676, .F. ) ;
#12829 = FACE_OUTER_BOUND ( 'NONE', #22570, .T. ) ;
#12830 = EDGE_CURVE ( 'NONE', #5794, #20973, #5645, .T. ) ;
#12831 = DIRECTION ( 'NONE',  ( -0.000000000000000000, -0.000000000000000000, -1.000000000000000000 ) ) ;
#12832 = CARTESIAN_POINT ( 'NONE',  ( 2.454813078130514813E-15, 16.67999999999999972, 14.50000000000000000 ) ) ;
#12833 = CARTESIAN_POINT ( 'NONE',  ( 2.682529543899157876, 8.255977015246598327, 7.033165578109189298 ) ) ;
#12834 = ORIENTED_EDGE ( 'NONE', *, *, #4035, .F. ) ;
#12835 = VERTEX_POINT ( 'NONE', #20896 ) ;
#12836 = VERTEX_POINT ( 'NONE', #13069 ) ;
#12837 = AXIS2_PLACEMENT_3D ( 'NONE', #23648, #17907, #16057 ) ;
#12838 = AXIS2_PLACEMENT_3D ( 'NONE', #1938, #23693, #5126 ) ;
#12839 = ORIENTED_EDGE ( 'NONE', *, *, #9846, .T. ) ;
#12840 = DIRECTION ( 'NONE',  ( 1.000000000000000000, 0.000000000000000000, 0.000000000000000000 ) ) ;
#12841 = CARTESIAN_POINT ( 'NONE',  ( -7.685661446562381371, 5.583959896777970222, 10.00674201446023481 ) ) ;
#12842 = ORIENTED_EDGE ( 'NONE', *, *, #21704, .F. ) ;
#12843 = ORIENTED_EDGE ( 'NONE', *, *, #12777, .F. ) ;
#12844 = LINE ( 'NONE', #23737, #9491 ) ;
#12845 = VERTEX_POINT ( 'NONE', #512 ) ;
#12846 = DIRECTION ( 'NONE',  ( 0.7071067811865469066, 8.659560562354925463E-17, -0.7071067811865481278 ) ) ;
#12847 = DIRECTION ( 'NONE',  ( -0.8757121056631640421, 0.4828336235133042775, 0.000000000000000000 ) ) ;
#12848 = DIRECTION ( 'NONE',  ( 0.000000000000000000, -1.000000000000000000, 0.000000000000000000 ) ) ;
#12849 = CARTESIAN_POINT ( 'NONE',  ( 23.00000000000000000, 14.21257171757157245, 6.139082186136624486 ) ) ;
#12850 = DIRECTION ( 'NONE',  ( -1.000000000000000000, 0.000000000000000000, 0.000000000000000000 ) ) ;
#12851 = CIRCLE ( 'NONE', #15191, 17.87500000001787726 ) ;
#12852 = DIRECTION ( 'NONE',  ( 0.5735764363510427177, -0.8191520442889941300, 1.003171929053527705E-16 ) ) ;
#12853 = EDGE_CURVE ( 'NONE', #11189, #18498, #14175, .T. ) ;
#12854 = CARTESIAN_POINT ( 'NONE',  ( 40.66734255040738333, 26.56420859267091217, -3.000000000000000000 ) ) ;
#12855 = EDGE_CURVE ( 'NONE', #18108, #556, #14941, .T. ) ;
#12856 = FACE_OUTER_BOUND ( 'NONE', #11935, .T. ) ;
#12857 = ORIENTED_EDGE ( 'NONE', *, *, #20803, .F. ) ;
#12858 = ORIENTED_EDGE ( 'NONE', *, *, #11379, .F. ) ;
#12859 = CARTESIAN_POINT ( 'NONE',  ( 5.365059087799946447, -7.384370330706356178, 10.33316557810919001 ) ) ;
#12860 = ORIENTED_EDGE ( 'NONE', *, *, #3295, .F. ) ;
#12861 = APPLICATION_PROTOCOL_DEFINITION ( 'draft international standard', 'automotive_design', 1998, #17740 ) ;
#12862 = CYLINDRICAL_SURFACE ( 'NONE', #9708, 5.000000000000000888 ) ;
#12863 = ORIENTED_EDGE ( 'NONE', *, *, #20385, .T. ) ;
#12864 = ORIENTED_EDGE ( 'NONE', *, *, #16785, .T. ) ;
#12865 = DIRECTION ( 'NONE',  ( -1.000000000000000000, 0.000000000000000000, 0.000000000000000000 ) ) ;
#12866 = CARTESIAN_POINT ( 'NONE',  ( -7.022953521755574080, 5.102474405759713783, -11.43316557810918965 ) ) ;
#12867 = AXIS2_PLACEMENT_3D ( 'NONE', #22968, #13811, #23673 ) ;
#12868 = ORIENTED_EDGE ( 'NONE', *, *, #3971, .T. ) ;
#12869 = CARTESIAN_POINT ( 'NONE',  ( 71.96568270381689558, -9.244463733058732095E-30, 5.000000000000007994 ) ) ;
#12870 = DIRECTION ( 'NONE',  ( 0.000000000000000000, -1.000000000000000000, 0.000000000000000000 ) ) ;
#12871 = CARTESIAN_POINT ( 'NONE',  ( -40.00000000000000000, -28.80990663662251450, 12.00000000000000000 ) ) ;
#12872 = FACE_OUTER_BOUND ( 'NONE', #18261, .T. ) ;
#12873 = CARTESIAN_POINT ( 'NONE',  ( 31.10231664966676135, 45.36128193761570770, 27.00000000000000000 ) ) ;
#12874 = ORIENTED_EDGE ( 'NONE', *, *, #1464, .F. ) ;
#12875 = CARTESIAN_POINT ( 'NONE',  ( 41.99999999999999289, 25.93535998569253920, 27.00000000000000000 ) ) ;
#12876 = EDGE_CURVE ( 'NONE', #4529, #6633, #7920, .T. ) ;
#12877 = ORIENTED_EDGE ( 'NONE', *, *, #14158, .T. ) ;
#12878 = ORIENTED_EDGE ( 'NONE', *, *, #17521, .F. ) ;
#12879 = CARTESIAN_POINT ( 'NONE',  ( 23.00000000000000000, 6.242160243097161221, 9.879763041175145588 ) ) ;
#12880 = CARTESIAN_POINT ( 'NONE',  ( 9.500000000000000000, 0.000000000000000000, -12.00000000000000000 ) ) ;
#12881 = CARTESIAN_POINT ( 'NONE',  ( 5.378177448618336243, 0.000000000000000000, 0.000000000000000000 ) ) ;
#12882 = PRESENTATION_STYLE_ASSIGNMENT (( #3506 ) ) ;
#12883 = EDGE_CURVE ( 'NONE', #17625, #12918, #3658, .T. ) ;
#12884 = DIRECTION ( 'NONE',  ( 1.000000000000000000, 1.224606353822377258E-16, 0.000000000000000000 ) ) ;
#12885 = ADVANCED_FACE ( 'NONE', ( #19170 ), #546, .T. ) ;
#12886 = DIRECTION ( 'NONE',  ( 0.000000000000000000, -1.000000000000000000, 0.000000000000000000 ) ) ;
#12887 = EDGE_CURVE ( 'NONE', #5160, #3619, #11034, .T. ) ;
#12888 = ADVANCED_FACE ( 'NONE', ( #10381 ), #21619, .F. ) ;
#12889 = CARTESIAN_POINT ( 'NONE',  ( -31.74999999999995737, 0.000000000000000000, 5.000000000000000888 ) ) ;
#12890 = VERTEX_POINT ( 'NONE', #8166 ) ;
#12891 = ORIENTED_EDGE ( 'NONE', *, *, #8061, .T. ) ;
#12892 = AXIS2_PLACEMENT_3D ( 'NONE', #20235, #9591, #337 ) ;
#12893 = CARTESIAN_POINT ( 'NONE',  ( -7.685661446562381371, 5.583959896777970222, 8.006742014460233037 ) ) ;
#12894 = EDGE_LOOP ( 'NONE', ( #7380, #16592, #20409, #1173 ) ) ;
#12895 = ORIENTED_EDGE ( 'NONE', *, *, #5723, .T. ) ;
#12896 =( NAMED_UNIT ( * ) PLANE_ANGLE_UNIT ( ) SI_UNIT ( $, .RADIAN. ) );
#12897 = CARTESIAN_POINT ( 'NONE',  ( 31.10231664966676846, 45.36128193761570770, 0.000000000000000000 ) ) ;
#12898 = CARTESIAN_POINT ( 'NONE',  ( -45.00000000000001421, 50.99999999999992184, 0.000000000000000000 ) ) ;
#12899 = CARTESIAN_POINT ( 'NONE',  ( 0.000000000000000000, 12.02595010061972403, -13.22467954916274913 ) ) ;
#12900 = DIRECTION ( 'NONE',  ( -1.000000000000000000, -0.000000000000000000, -0.000000000000000000 ) ) ;
#12901 = CARTESIAN_POINT ( 'NONE',  ( 10.40000000000000036, 0.000000000000000000, 0.000000000000000000 ) ) ;
#12902 = CARTESIAN_POINT ( 'NONE',  ( 0.000000000000000000, 1.785035801044272647E-15, -14.42592346043842255 ) ) ;
#12903 = CARTESIAN_POINT ( 'NONE',  ( -6.822232771736904647E-13, 9.988891130263535700, -10.55958914175814201 ) ) ;
#12904 = EDGE_CURVE ( 'NONE', #20508, #9321, #8051, .T. ) ;
#12905 = AXIS2_PLACEMENT_3D ( 'NONE', #21998, #5399, #11095 ) ;
#12906 = DIRECTION ( 'NONE',  ( 1.000000000000000000, 0.000000000000000000, -0.000000000000000000 ) ) ;
#12907 =( NAMED_UNIT ( * ) PLANE_ANGLE_UNIT ( ) SI_UNIT ( $, .RADIAN. ) );
#12908 = VECTOR ( 'NONE', #19481, 1000.000000000000000 ) ;
#12909 = CARTESIAN_POINT ( 'NONE',  ( 9.330908268522616567, -1.784418920661929642, -11.99999999999998934 ) ) ;
#12910 = CARTESIAN_POINT ( 'NONE',  ( 35.99999999999999289, -51.00000000000000711, 12.50000000000000000 ) ) ;
#12911 = FACE_OUTER_BOUND ( 'NONE', #21721, .T. ) ;
#12912 = EDGE_CURVE ( 'NONE', #4703, #16945, #20091, .T. ) ;
#12913 = CARTESIAN_POINT ( 'NONE',  ( 7.022953521755574080, -5.102474405759714671, -10.43316557810918788 ) ) ;
#12914 = EDGE_CURVE ( 'NONE', #21366, #20685, #6725, .T. ) ;
#12915 = CARTESIAN_POINT ( 'NONE',  ( 0.000000000000000000, 0.000000000000000000, 6.000000000000000000 ) ) ;
#12916 = VERTEX_POINT ( 'NONE', #4665 ) ;
#12917 = DIRECTION ( 'NONE',  ( -1.000000000000000000, -1.224606353822377258E-16, -0.000000000000000000 ) ) ;
#12918 = VERTEX_POINT ( 'NONE', #23342 ) ;
#12919 = DIRECTION ( 'NONE',  ( 0.000000000000000000, 0.000000000000000000, -1.000000000000000000 ) ) ;
#12920 = DIRECTION ( 'NONE',  ( -1.000000000000000000, -1.224606353822377258E-16, -0.000000000000000000 ) ) ;
#12921 = VERTEX_POINT ( 'NONE', #6495 ) ;
#12922 = CARTESIAN_POINT ( 'NONE',  ( 73.12522638709218370, 7.562528597612068045E-15, 0.000000000000000000 ) ) ;
#12923 = CARTESIAN_POINT ( 'NONE',  ( 19.85000000000000142, 16.67999999999999972, 14.50000000000000000 ) ) ;
#12924 = DIRECTION ( 'NONE',  ( -1.000000000000000000, -0.000000000000000000, -0.000000000000000000 ) ) ;
#12925 = MECHANICAL_DESIGN_GEOMETRIC_PRESENTATION_REPRESENTATION (  '', ( #7081 ), #5911 ) ;
#12926 = CIRCLE ( 'NONE', #5152, 5.000000000000007994 ) ;
#12927 = AXIS2_PLACEMENT_3D ( 'NONE', #10237, #17693, #8420 ) ;
#12928 = CARTESIAN_POINT ( 'NONE',  ( 0.000000000000000000, 45.00000000000000000, -3.000000000000000000 ) ) ;
#12929 = VECTOR ( 'NONE', #23437, 1000.000000000000114 ) ;
#12930 = FACE_OUTER_BOUND ( 'NONE', #1484, .T. ) ;
#12931 = CARTESIAN_POINT ( 'NONE',  ( -2.935661446562617183, 9.035036904803758873, -10.65958914175814343 ) ) ;
#12932 = ORIENTED_EDGE ( 'NONE', *, *, #6879, .T. ) ;
#12933 = ORIENTED_EDGE ( 'NONE', *, *, #16262, .T. ) ;
#12934 = CARTESIAN_POINT ( 'NONE',  ( -41.00000000000000000, 4.000000000000000888, 10.49999999999999822 ) ) ;
#12935 = ORIENTED_EDGE ( 'NONE', *, *, #20288, .T. ) ;
#12936 = LINE ( 'NONE', #3330, #2675 ) ;
#12937 = CONICAL_SURFACE ( 'NONE', #16067, 4.057500000000000107, 1.047197551196593857 ) ;
#12938 = VECTOR ( 'NONE', #1248, 1000.000000000000000 ) ;
#12939 = ORIENTED_EDGE ( 'NONE', *, *, #4161, .F. ) ;
#12940 = EDGE_CURVE ( 'NONE', #4159, #9926, #19426, .T. ) ;
#12941 = CARTESIAN_POINT ( 'NONE',  ( 11.50000000000000000, -17.86986844953242937, 0.4282833139926494059 ) ) ;
#12942 = AXIS2_PLACEMENT_3D ( 'NONE', #18543, #22095, #9247 ) ;
#12943 = DIRECTION ( 'NONE',  ( -0.000000000000000000, -0.000000000000000000, -1.000000000000000000 ) ) ;
#12944 = CIRCLE ( 'NONE', #5552, 5.400000000000001243 ) ;
#12945 = FACE_OUTER_BOUND ( 'NONE', #22872, .T. ) ;
#12946 = ORIENTED_EDGE ( 'NONE', *, *, #8255, .F. ) ;
#12947 = AXIS2_PLACEMENT_3D ( 'NONE', #5292, #23611, #23480 ) ;
#12948 = CARTESIAN_POINT ( 'NONE',  ( -40.00000000000000000, 29.49999999999999645, 11.00000000000000000 ) ) ;
#12949 = CARTESIAN_POINT ( 'NONE',  ( 5.365059087799947335, -7.384370330706356178, 12.33316557810918823 ) ) ;
#12950 = DIRECTION ( 'NONE',  ( -0.000000000000000000, -0.000000000000000000, 1.000000000000000000 ) ) ;
#12951 = AXIS2_PLACEMENT_3D ( 'NONE', #13117, #18729, #9681 ) ;
#12952 =( BOUNDED_SURFACE ( )  B_SPLINE_SURFACE ( 1, 2, ( 
 ( #2567, #17439, #15591, #23055, #13783, #21231, #4534, #11939, #19405, #4616, #10184, #4862, #12391, #17412, #2529, #707, #6562, #3437, #17775, #7314, #23695, #18553, #12913, #1712, #3784, #5378, #16588, #10, #6968, #22333, #13038, #14753, #20501, #1492, #5257, #18422, #3657, #12550, #11191, #1369, #14391, #21847, #23799, #20023, #3306, #14503, #12683, #18308, #1592, #4154, #361, #2308, #479, #22937, #4270, #15473, #7895, #7535, #19142, #2422, #17310, #3895, #13649, #610, #9483, #7661, #6822, #23049, #13773, #3046, #2674, #10466, #21351, #19275, #17810, #14251, #8522, #19771, #21716, #12042, #17432, #11799, #4886, #15964, #23180, #12300, #10347, #17674, #17544, #23424, #2559, #17928, #21221, #14132, #16079, #4527, #14020 ),
 ( #1215, #8626, #730, #11932, #8264, #975, #21465, #19399, #6589, #8139, #10091, #842, #15715, #6463, #13909, #4640, #19512, #2792, #10213, #8398, #8982, #16426, #12774, #18524, #20234, #19876, #23889, #10920, #16558, #14365, #20345, #3628, #11046, #1340, #10577, #1810, #16682, #21823, #3152, #18170, #8878, #16317, #9812, #3841, #2249, #18590, #17571, #7929, #4667, #4556, #19428, #2705, #2592, #10003, #10119, #644, #874, #19308, #6238, #13937, #17460, #8301, #2335, #13678, #7799, #6124, #15380, #4299, #23217, #21378, #13808, #759, #9748, #17205, #8053, #15498, #15612, #6498, #513, #21008, #21118, #8168, #11591, #23077, #6366, #11960, #21259, #22850, #19062, #22713, #10255, #11701, #2458, #13565, #4425, #9884, #22966 ) ),
 .UNSPECIFIED., .F., .F., .T. ) 
 B_SPLINE_SURFACE_WITH_KNOTS ( ( 2, 2 ),
 ( 3, 2, 2, 2, 2, 2, 2, 2, 2, 2, 2, 2, 2, 2, 2, 2, 2, 2, 2, 2, 2, 2, 2, 2, 2, 2, 2, 2, 2, 2, 2, 2, 2, 2, 2, 2, 2, 2, 2, 2, 2, 2, 2, 2, 2, 2, 2, 2, 3 ),
 ( 0.000000000000000000, 1.000000000000000000 ),
 ( 0.000000000000000000, 0.02000000000000000042, 0.04000000000000000083, 0.05999999999999999778, 0.08000000000000000167, 0.1000000000000000056, 0.1199999999999999956, 0.1400000000000000133, 0.1600000000000000033, 0.1799999999999999933, 0.2000000000000000111, 0.2200000000000000011, 0.2399999999999999911, 0.2600000000000000089, 0.2800000000000000266, 0.2999999999999999889, 0.3200000000000000067, 0.3400000000000000244, 0.3599999999999999867, 0.3800000000000000044, 0.4000000000000000222, 0.4199999999999999845, 0.4400000000000000022, 0.4600000000000000200, 0.4799999999999999822, 0.5000000000000000000, 0.5200000000000000178, 0.5400000000000000355, 0.5600000000000000533, 0.5799999999999999600, 0.5999999999999999778, 0.6199999999999999956, 0.6400000000000000133, 0.6600000000000000311, 0.6800000000000000488, 0.6999999999999999556, 0.7199999999999999734, 0.7399999999999999911, 0.7600000000000000089, 0.7800000000000000266, 0.8000000000000000444, 0.8199999999999999512, 0.8399999999999999689, 0.8599999999999999867, 0.8800000000000000044, 0.9000000000000000222, 0.9200000000000000400, 0.9399999999999999467, 0.9500000000000000666 ),
 .UNSPECIFIED. ) 
 GEOMETRIC_REPRESENTATION_ITEM ( )  RATIONAL_B_SPLINE_SURFACE ( (
 ( 1.000000000000000000, 0.9510565162951535312, 1.000000000000000000, 0.9510565162951535312, 1.000000000000000000, 0.9510565162951535312, 1.000000000000000000, 0.9510565162951535312, 1.000000000000000000, 0.9510565162951535312, 1.000000000000000000, 0.9510565162951535312, 1.000000000000000000, 0.9510565162951535312, 1.000000000000000000, 0.9510565162951535312, 1.000000000000000000, 0.9510565162951535312, 1.000000000000000000, 0.9510565162951535312, 1.000000000000000000, 0.9510565162951535312, 1.000000000000000000, 0.9510565162951535312, 1.000000000000000000, 0.9510565162951535312, 1.000000000000000000, 0.9510565162951535312, 1.000000000000000000, 0.9510565162951535312, 1.000000000000000000, 0.9510565162951535312, 1.000000000000000000, 0.9510565162951535312, 1.000000000000000000, 0.9510565162951535312, 1.000000000000000000, 0.9510565162951535312, 1.000000000000000000, 0.9510565162951535312, 1.000000000000000000, 0.9510565162951535312, 1.000000000000000000, 0.9510565162951535312, 1.000000000000000000, 0.9510565162951535312, 1.000000000000000000, 0.9510565162951535312, 1.000000000000000000, 0.9510565162951535312, 1.000000000000000000, 0.9510565162951535312, 1.000000000000000000, 0.9510565162951535312, 1.000000000000000000, 0.9510565162951535312, 1.000000000000000000, 0.9510565162951535312, 1.000000000000000000, 0.9510565162951535312, 1.000000000000000000, 0.9510565162951535312, 1.000000000000000000, 0.9510565162951535312, 1.000000000000000000, 0.9510565162951535312, 1.000000000000000000, 0.9510565162951535312, 1.000000000000000000, 0.9510565162951535312, 1.000000000000000000, 0.9510565162951535312, 1.000000000000000000, 0.9510565162951535312, 1.000000000000000000, 0.9510565162951535312, 1.000000000000000000, 0.9510565162951535312, 1.000000000000000000, 0.9510565162951535312, 1.000000000000000000, 0.9510565162951535312, 1.000000000000000000, 0.9510565162951535312, 1.000000000000000000, 0.9510565162951535312, 1.000000000000000000, 0.9510565162951535312, 1.000000000000000000, 0.9510565162951535312, 1.000000000000000000, 0.9510565162951535312, 1.000000000000000000, 0.9510565162951535312, 1.000000000000000000, 0.9755282581475764880, 0.9755282581475768211),
 ( 1.000000000000000000, 0.9510565162951535312, 1.000000000000000000, 0.9510565162951535312, 1.000000000000000000, 0.9510565162951535312, 1.000000000000000000, 0.9510565162951535312, 1.000000000000000000, 0.9510565162951535312, 1.000000000000000000, 0.9510565162951535312, 1.000000000000000000, 0.9510565162951535312, 1.000000000000000000, 0.9510565162951535312, 1.000000000000000000, 0.9510565162951535312, 1.000000000000000000, 0.9510565162951535312, 1.000000000000000000, 0.9510565162951535312, 1.000000000000000000, 0.9510565162951535312, 1.000000000000000000, 0.9510565162951535312, 1.000000000000000000, 0.9510565162951535312, 1.000000000000000000, 0.9510565162951535312, 1.000000000000000000, 0.9510565162951535312, 1.000000000000000000, 0.9510565162951535312, 1.000000000000000000, 0.9510565162951535312, 1.000000000000000000, 0.9510565162951535312, 1.000000000000000000, 0.9510565162951535312, 1.000000000000000000, 0.9510565162951535312, 1.000000000000000000, 0.9510565162951535312, 1.000000000000000000, 0.9510565162951535312, 1.000000000000000000, 0.9510565162951535312, 1.000000000000000000, 0.9510565162951535312, 1.000000000000000000, 0.9510565162951535312, 1.000000000000000000, 0.9510565162951535312, 1.000000000000000000, 0.9510565162951535312, 1.000000000000000000, 0.9510565162951535312, 1.000000000000000000, 0.9510565162951535312, 1.000000000000000000, 0.9510565162951535312, 1.000000000000000000, 0.9510565162951535312, 1.000000000000000000, 0.9510565162951535312, 1.000000000000000000, 0.9510565162951535312, 1.000000000000000000, 0.9510565162951535312, 1.000000000000000000, 0.9510565162951535312, 1.000000000000000000, 0.9510565162951535312, 1.000000000000000000, 0.9510565162951535312, 1.000000000000000000, 0.9510565162951535312, 1.000000000000000000, 0.9510565162951535312, 1.000000000000000000, 0.9510565162951535312, 1.000000000000000000, 0.9510565162951535312, 1.000000000000000000, 0.9510565162951535312, 1.000000000000000000, 0.9510565162951535312, 1.000000000000000000, 0.9510565162951535312, 1.000000000000000000, 0.9510565162951535312, 1.000000000000000000, 0.9510565162951535312, 1.000000000000000000, 0.9755282581475764880, 0.9755282581475768211) ) ) 
 REPRESENTATION_ITEM ( '' )  SURFACE ( )  );
#12953 = CARTESIAN_POINT ( 'NONE',  ( 0.000000000000000000, -14.99147757894464306, 7.750000000000000000 ) ) ;
#12954 = VERTEX_POINT ( 'NONE', #14160 ) ;
#12955 = ORIENTED_EDGE ( 'NONE', *, *, #9611, .F. ) ;
#12956 = VECTOR ( 'NONE', #17769, 1000.000000000000000 ) ;
#12957 = CONTEXT_DEPENDENT_SHAPE_REPRESENTATION ( #20558, #8460 ) ;
#12958 = ORIENTED_EDGE ( 'NONE', *, *, #16586, .F. ) ;
#12959 = CIRCLE ( 'NONE', #4002, 5.099999999999996980 ) ;
#12960 = ADVANCED_FACE ( 'NONE', ( #17458 ), #16951, .F. ) ;
#12961 = AXIS2_PLACEMENT_3D ( 'NONE', #15149, #11243, #20793 ) ;
#12962 = CIRCLE ( 'NONE', #4027, 1.500000000000001332 ) ;
#12963 = DIRECTION ( 'NONE',  ( 0.000000000000000000, -1.000000000000000000, 0.000000000000000000 ) ) ;
#12964 = AXIS2_PLACEMENT_3D ( 'NONE', #3790, #20621, #18671 ) ;
#12965 = EDGE_CURVE ( 'NONE', #13276, #18469, #10117, .T. ) ;
#12966 = FACE_OUTER_BOUND ( 'NONE', #10989, .T. ) ;
#12967 = VECTOR ( 'NONE', #9470, 1000.000000000000114 ) ;
#12968 = ORIENTED_EDGE ( 'NONE', *, *, #3791, .F. ) ;
#12969 = DIRECTION ( 'NONE',  ( 1.000000000000000000, 0.000000000000000000, 0.000000000000000000 ) ) ;
#12970 = EDGE_CURVE ( 'NONE', #12205, #10649, #4919, .T. ) ;
#12971 = CARTESIAN_POINT ( 'NONE',  ( 76.03431729618309021, 7.562528597612068045E-15, 0.000000000000000000 ) ) ;
#12972 = FACE_BOUND ( 'NONE', #1058, .T. ) ;
#12973 = CARTESIAN_POINT ( 'NONE',  ( 20.85000000000000853, 15.03999999999999915, -27.00000000000000000 ) ) ;
#12974 = CARTESIAN_POINT ( 'NONE',  ( 41.00000000000000000, 5.999999999999986677, 11.00000000000000000 ) ) ;
#12975 = MECHANICAL_DESIGN_GEOMETRIC_PRESENTATION_REPRESENTATION (  '', ( #5989 ), #11801 ) ;
#12976 = CYLINDRICAL_SURFACE ( 'NONE', #11813, 1.000000000000000000 ) ;
#12977 = DIRECTION ( 'NONE',  ( -0.5735764363510517105, -0.8191520442889879128, 0.000000000000000000 ) ) ;
#12978 = AXIS2_PLACEMENT_3D ( 'NONE', #7500, #22650, #9334 ) ;
#12979 = CARTESIAN_POINT ( 'NONE',  ( 0.000000000000000000, 0.000000000000000000, 14.42592346043842255 ) ) ;
#12980 = VERTEX_POINT ( 'NONE', #10251 ) ;
#12981 = AXIS2_PLACEMENT_3D ( 'NONE', #8080, #21289, #22750 ) ;
#12982 = DIRECTION ( 'NONE',  ( -1.000000000000000000, 0.000000000000000000, 0.000000000000000000 ) ) ;
#12983 = VERTEX_POINT ( 'NONE', #23075 ) ;
#12984 = CIRCLE ( 'NONE', #4046, 1.000000000000000888 ) ;
#12985 = CONICAL_SURFACE ( 'NONE', #13376, 5.025000000000002132, 0.7853981633974482790 ) ;
#12986 = AXIS2_PLACEMENT_3D ( 'NONE', #11500, #9667, #14920 ) ;
#12987 = PRODUCT_CONTEXT ( 'NONE', #9439, 'mechanical' ) ;
#12988 = VERTEX_POINT ( 'NONE', #6363 ) ;
#12989 = VERTEX_POINT ( 'NONE', #17707 ) ;
#12990 = CARTESIAN_POINT ( 'NONE',  ( -7.561939491010498671, 5.750397476200742375, -11.99999999999999822 ) ) ;
#12991 = CARTESIAN_POINT ( 'NONE',  ( -2.682529543899159208, -8.255977015246598327, -10.03316557810918930 ) ) ;
#12992 = EDGE_CURVE ( 'NONE', #13157, #4844, #8777, .T. ) ;
#12993 = EDGE_LOOP ( 'NONE', ( #4158, #19457, #22377, #17178, #4985 ) ) ;
#12994 = DIRECTION ( 'NONE',  ( 0.000000000000000000, 0.000000000000000000, 1.000000000000000000 ) ) ;
#12995 = CARTESIAN_POINT ( 'NONE',  ( 87.67068093254673045, 5.000000000000015099, 0.000000000000000000 ) ) ;
#12996 = EDGE_CURVE ( 'NONE', #10733, #11221, #3727, .T. ) ;
#12997 = EDGE_CURVE ( 'NONE', #18651, #7449, #13910, .T. ) ;
#12998 = DIRECTION ( 'NONE',  ( -0.000000000000000000, 0.000000000000000000, 1.000000000000000000 ) ) ;
#12999 = AXIS2_PLACEMENT_3D ( 'NONE', #15124, #18940, #17203 ) ;
#13000 = DIRECTION ( 'NONE',  ( 1.000000000000000000, -0.000000000000000000, -0.000000000000000000 ) ) ;
#13001 = VERTEX_POINT ( 'NONE', #6969 ) ;
#13002 = PLANE ( 'NONE',  #10606 ) ;
#13003 = ORIENTED_EDGE ( 'NONE', *, *, #1859, .T. ) ;
#13004 = AXIS2_PLACEMENT_3D ( 'NONE', #10851, #10389, #17846 ) ;
#13005 = VERTEX_POINT ( 'NONE', #10841 ) ;
#13006 = DIRECTION ( 'NONE',  ( -0.000000000000000000, -0.000000000000000000, -1.000000000000000000 ) ) ;
#13007 = CARTESIAN_POINT ( 'NONE',  ( -9.500000000000000000, -6.482511860946779655E-13, -9.059589141758143782 ) ) ;
#13008 = AXIS2_PLACEMENT_3D ( 'NONE', #23870, #1905, #22414 ) ;
#13009 = CARTESIAN_POINT ( 'NONE',  ( 40.00000000000000000, -28.80990663662251450, 0.000000000000000000 ) ) ;
#13010 = CARTESIAN_POINT ( 'NONE',  ( 15.56475192642548322, 5.220978644676159242, -7.947934502462939754 ) ) ;
#13011 = AXIS2_PLACEMENT_3D ( 'NONE', #10345, #17925, #728 ) ;
#13012 = DIRECTION ( 'NONE',  ( -0.000000000000000000, -0.000000000000000000, -1.000000000000000000 ) ) ;
#13013 = DIRECTION ( 'NONE',  ( -1.000000000000000000, -0.000000000000000000, -0.000000000000000000 ) ) ;
#13014 = CYLINDRICAL_SURFACE ( 'NONE', #1605, 5.000000000000000888 ) ;
#13015 = ORIENTED_EDGE ( 'NONE', *, *, #4628, .T. ) ;
#13016 = EDGE_LOOP ( 'NONE', ( #960, #23073, #20053, #13636 ) ) ;
#13017 = CARTESIAN_POINT ( 'NONE',  ( 2.935661446562616295, -9.035036904803758873, 10.80674201446023197 ) ) ;
#13018 = ORIENTED_EDGE ( 'NONE', *, *, #5413, .F. ) ;
#13019 = PRODUCT_RELATED_PRODUCT_CATEGORY ( 'part', '', ( #9573 ) ) ;
#13020 = ORIENTED_EDGE ( 'NONE', *, *, #11636, .T. ) ;
#13021 = CIRCLE ( 'NONE', #15764, 23.85000000000000142 ) ;
#13022 = EDGE_CURVE ( 'NONE', #23407, #12319, #18919, .T. ) ;
#13023 = VECTOR ( 'NONE', #17114, 1000.000000000000114 ) ;
#13024 = AXIS2_PLACEMENT_3D ( 'NONE', #17588, #4683, #1144 ) ;
#13025 = EDGE_CURVE ( 'NONE', #17812, #14877, #10730, .T. ) ;
#13026 = AXIS2_PLACEMENT_3D ( 'NONE', #11033, #211, #1907 ) ;
#13027 = DIRECTION ( 'NONE',  ( 0.000000000000000000, -1.000000000000000000, 0.000000000000000000 ) ) ;
#13028 = CARTESIAN_POINT ( 'NONE',  ( 62.94340820527399671, 7.562528597612068045E-15, 0.000000000000000000 ) ) ;
#13029 = ADVANCED_FACE ( 'NONE', ( #18311 ), #11485, .T. ) ;
#13030 = EDGE_CURVE ( 'NONE', #3826, #12366, #18423, .T. ) ;
#13031 = CARTESIAN_POINT ( 'NONE',  ( 72.54545454545454675, 7.491529369508391930E-15, 0.000000000000000000 ) ) ;
#13032 = DIRECTION ( 'NONE',  ( -0.000000000000000000, -0.000000000000000000, 1.000000000000000000 ) ) ;
#13033 = CARTESIAN_POINT ( 'NONE',  ( -17.59041996266972774, 9.500503876990130436, 0.4759723220310715375 ) ) ;
#13034 = CARTESIAN_POINT ( 'NONE',  ( -6.153822176767817416E-13, 9.500000000000000000, -3.706742014460231882 ) ) ;
#13035 = AXIS2_PLACEMENT_3D ( 'NONE', #6479, #855, #22950 ) ;
#13036 = AXIS2_PLACEMENT_3D ( 'NONE', #23578, #23802, #21976 ) ;
#13037 = CARTESIAN_POINT ( 'NONE',  ( 29.00000000000000000, -29.50000000000000355, 11.50000000000000000 ) ) ;
#13038 = CARTESIAN_POINT ( 'NONE',  ( -8.680847955711007202, -5.923547351154968927E-13, -9.633165578109188942 ) ) ;
#13039 = VECTOR ( 'NONE', #13761, 1000.000000000000000 ) ;
#13040 = DIRECTION ( 'NONE',  ( -1.000000000000000000, 0.000000000000000000, 0.000000000000000000 ) ) ;
#13041 = ORIENTED_EDGE ( 'NONE', *, *, #10101, .F. ) ;
#13042 = DIRECTION ( 'NONE',  ( 1.000000000000000000, 0.000000000000000000, 0.000000000000000000 ) ) ;
#13043 = AXIS2_PLACEMENT_3D ( 'NONE', #19808, #2829, #14054 ) ;
#13044 = ORIENTED_EDGE ( 'NONE', *, *, #13561, .T. ) ;
#13045 = CARTESIAN_POINT ( 'NONE',  ( 64.39795365981944997, -5.000000000000000000, 6.123233995736775157E-16 ) ) ;
#13046 = ORIENTED_EDGE ( 'NONE', *, *, #13505, .T. ) ;
#13047 =( NAMED_UNIT ( * ) PLANE_ANGLE_UNIT ( ) SI_UNIT ( $, .RADIAN. ) );
#13048 = AXIS2_PLACEMENT_3D ( 'NONE', #22964, #8430, #2590 ) ;
#13049 = VECTOR ( 'NONE', #13895, 1000.000000000000000 ) ;
#13050 = CYLINDRICAL_SURFACE ( 'NONE', #12243, 11.68650000001168721 ) ;
#13051 = EDGE_CURVE ( 'NONE', #22408, #21057, #6854, .T. ) ;
#13052 = CARTESIAN_POINT ( 'NONE',  ( 0.000000000000000000, 15.50000000000000000, 14.70000000000000284 ) ) ;
#13053 = CARTESIAN_POINT ( 'NONE',  ( 23.00000000000000000, 3.378881074890460745, -11.18737882312118082 ) ) ;
#13054 = DIRECTION ( 'NONE',  ( 1.000000000000000000, 0.000000000000000000, -0.000000000000000000 ) ) ;
#13055 =( REPRESENTATION_RELATIONSHIP ('NONE','NONE', #21748, #5350 ) REPRESENTATION_RELATIONSHIP_WITH_TRANSFORMATION ( #17099 )SHAPE_REPRESENTATION_RELATIONSHIP( ) );
#13056 = EDGE_CURVE ( 'NONE', #7931, #5307, #14211, .T. ) ;
#13057 = ADVANCED_FACE ( 'NONE', ( #3176 ), #3070, .T. ) ;
#13058 = DIRECTION ( 'NONE',  ( -0.000000000000000000, -0.000000000000000000, -1.000000000000000000 ) ) ;
#13059 = CARTESIAN_POINT ( 'NONE',  ( -5.871322893124554021, 8.081182679343978492, -6.759589141758143072 ) ) ;
#13060 = ORIENTED_EDGE ( 'NONE', *, *, #2609, .F. ) ;
#13061 = ORIENTED_EDGE ( 'NONE', *, *, #8381, .T. ) ;
#13062 = LINE ( 'NONE', #7434, #13039 ) ;
#13063 = ORIENTED_EDGE ( 'NONE', *, *, #14281, .T. ) ;
#13064 = LINE ( 'NONE', #5864, #18050 ) ;
#13065 = CARTESIAN_POINT ( 'NONE',  ( -41.00000000000000000, -4.000000000000000888, 8.500000000000000000 ) ) ;
#13066 = AXIS2_PLACEMENT_3D ( 'NONE', #11193, #3896, #3659 ) ;
#13067 = ORIENTED_EDGE ( 'NONE', *, *, #4266, .T. ) ;
#13068 = DIRECTION ( 'NONE',  ( -0.000000000000000000, -0.000000000000000000, -1.000000000000000000 ) ) ;
#13069 = CARTESIAN_POINT ( 'NONE',  ( 63.23840997654417606, 5.000000000000007105, 6.123233995736765296E-16 ) ) ;
#13070 = CARTESIAN_POINT ( 'NONE',  ( 70.51113724927145654, -9.244463733058732095E-30, 5.000000000000007994 ) ) ;
#13071 = ORIENTED_EDGE ( 'NONE', *, *, #17841, .T. ) ;
#13072 = DIRECTION ( 'NONE',  ( -1.000000000000000000, -1.224606353822377258E-16, -0.000000000000000000 ) ) ;
#13073 = DIRECTION ( 'NONE',  ( -1.000000000000000000, -2.600433232233976523E-16, 0.000000000000000000 ) ) ;
#13074 = AXIS2_PLACEMENT_3D ( 'NONE', #6979, #2831, #17965 ) ;
#13075 = FACE_OUTER_BOUND ( 'NONE', #13828, .T. ) ;
#13076 = AXIS2_PLACEMENT_3D ( 'NONE', #22201, #9345, #3770 ) ;
#13077 = CYLINDRICAL_SURFACE ( 'NONE', #3984, 1.000000000000000888 ) ;
#13078 = VERTEX_POINT ( 'NONE', #4918 ) ;
#13079 = PRODUCT ( 'End Plate', 'End Plate', '', ( #1661 ) ) ;
#13080 = VERTEX_POINT ( 'NONE', #5127 ) ;
#13081 = VECTOR ( 'NONE', #8774, 1000.000000000000000 ) ;
#13082 = ORIENTED_EDGE ( 'NONE', *, *, #19031, .T. ) ;
#13083 = AXIS2_PLACEMENT_3D ( 'NONE', #3564, #5518, #18230 ) ;
#13084 = ITEM_DEFINED_TRANSFORMATION ( 'NONE', 'NONE', #23265,  #8005 ) ;
#13085 = EDGE_LOOP ( 'NONE', ( #1689, #19667 ) ) ;
#13086 = LINE ( 'NONE', #11121, #9936 ) ;
#13087 = EDGE_CURVE ( 'NONE', #9263, #8782, #2547, .T. ) ;
#13088 = EDGE_CURVE ( 'NONE', #13963, #11994, #9013, .T. ) ;
#13089 = ORIENTED_EDGE ( 'NONE', *, *, #14406, .F. ) ;
#13090 = CIRCLE ( 'NONE', #1036, 1.000000000000000888 ) ;
#13091 = CARTESIAN_POINT ( 'NONE',  ( -28.73477696352898292, 42.73830357953205805, -1.500000000000000000 ) ) ;
#13092 = VERTEX_POINT ( 'NONE', #19799 ) ;
#13093 = DIRECTION ( 'NONE',  ( -1.000000000000000000, -1.224606353822377258E-16, -0.000000000000000000 ) ) ;
#13094 = PRODUCT_DEFINITION_FORMATION_WITH_SPECIFIED_SOURCE ( 'ANY', '', #10410, .NOT_KNOWN. ) ;
#13095 = AXIS2_PLACEMENT_3D ( 'NONE', #6569, #6196, #14003 ) ;
#13096 = CARTESIAN_POINT ( 'NONE',  ( 87.67068093254673045, 7.562528597612068045E-15, 0.000000000000000000 ) ) ;
#13097 = CARTESIAN_POINT ( 'NONE',  ( -5.799656021750657521E-13, 8.953898637140671468, -2.941973432658839371 ) ) ;
#13098 = CIRCLE ( 'NONE', #6490, 21.85000000000000142 ) ;
#13099 = CARTESIAN_POINT ( 'NONE',  ( -33.24999999999999289, -29.50000000000000000, -3.000000000000000000 ) ) ;
#13100 = CARTESIAN_POINT ( 'NONE',  ( 44.99999999999998579, 50.99999999999992184, 12.50000000000000000 ) ) ;
#13101 = VERTEX_POINT ( 'NONE', #14642 ) ;
#13102 = ORIENTED_EDGE ( 'NONE', *, *, #20639, .F. ) ;
#13103 = FACE_OUTER_BOUND ( 'NONE', #465, .T. ) ;
#13104 = CARTESIAN_POINT ( 'NONE',  ( 87.09090909090909349, -4.172000000000000597, 0.000000000000000000 ) ) ;
#13105 = EDGE_CURVE ( 'NONE', #20508, #10567, #4118, .T. ) ;
#13106 = DIRECTION ( 'NONE',  ( 0.000000000000000000, 0.000000000000000000, -1.000000000000000000 ) ) ;
#13107 = VERTEX_POINT ( 'NONE', #16456 ) ;
#13108 = CARTESIAN_POINT ( 'NONE',  ( -2.682529543899159208, -8.255977015246598327, 6.033165578109189298 ) ) ;
#13109 = VERTEX_POINT ( 'NONE', #7316 ) ;
#13110 = EDGE_CURVE ( 'NONE', #12890, #732, #10491, .T. ) ;
#13111 = CIRCLE ( 'NONE', #18192, 1.999999999999994449 ) ;
#13112 = PRODUCT_CONTEXT ( 'NONE', #21484, 'mechanical' ) ;
#13113 = DIRECTION ( 'NONE',  ( -1.000000000000000000, -0.000000000000000000, -0.000000000000000000 ) ) ;
#13114 = EDGE_LOOP ( 'NONE', ( #23833, #12134, #18129, #12858 ) ) ;
#13115 = ORIENTED_EDGE ( 'NONE', *, *, #11860, .F. ) ;
#13116 = EDGE_CURVE ( 'NONE', #13806, #14151, #22429, .T. ) ;
#13117 = CARTESIAN_POINT ( 'NONE',  ( 88.54545454545454675, 7.491529369508391930E-15, 0.000000000000000000 ) ) ;
#13118 = CARTESIAN_POINT ( 'NONE',  ( -8.680847955710813579, -2.820578480814258437, -11.73316557810918859 ) ) ;
#13119 = CARTESIAN_POINT ( 'NONE',  ( 58.87477361290780919, 7.420530141404717394E-15, 0.000000000000000000 ) ) ;
#13120 = ORIENTED_EDGE ( 'NONE', *, *, #2297, .T. ) ;
#13121 = CARTESIAN_POINT ( 'NONE',  ( 0.3000000000000023204, 0.000000000000000000, 9.725923461386809521 ) ) ;
#13122 = DIRECTION ( 'NONE',  ( -0.8757121056631640421, -0.4828336235133042775, -0.000000000000000000 ) ) ;
#13123 = CARTESIAN_POINT ( 'NONE',  ( 77.78386452199872281, 5.000000000000025757, 6.123233995736788962E-16 ) ) ;
#13124 = FACE_OUTER_BOUND ( 'NONE', #4378, .T. ) ;
#13125 = EDGE_LOOP ( 'NONE', ( #18848, #11690, #3105, #2237 ) ) ;
#13126 = DIRECTION ( 'NONE',  ( -1.000000000000000000, -1.224606353822377258E-16, -0.000000000000000000 ) ) ;
#13127 = VERTEX_POINT ( 'NONE', #14504 ) ;
#13128 = ORIENTED_EDGE ( 'NONE', *, *, #18001, .F. ) ;
#13129 = CARTESIAN_POINT ( 'NONE',  ( 0.000000000000000000, -45.00000000000000000, -26.97499999999999432 ) ) ;
#13130 = CARTESIAN_POINT ( 'NONE',  ( 41.00000000000000000, -6.000000000000015099, 11.00000000000000000 ) ) ;
#13131 = DIRECTION ( 'NONE',  ( -1.000000000000000000, 0.000000000000000000, 0.000000000000000000 ) ) ;
#13132 = LINE ( 'NONE', #334, #1366 ) ;
#13133 = DIRECTION ( 'NONE',  ( -0.8571673007021116675, 1.049727191138617833E-16, 0.5150380749100552658 ) ) ;
#13134 = CARTESIAN_POINT ( 'NONE',  ( -2.682529543899159208, -8.255977015246598327, -12.03316557810918930 ) ) ;
#13135 = ORIENTED_EDGE ( 'NONE', *, *, #7733, .F. ) ;
#13136 = ORIENTED_EDGE ( 'NONE', *, *, #7984, .F. ) ;
#13137 = EDGE_CURVE ( 'NONE', #12890, #13474, #20485, .T. ) ;
#13138 = ORIENTED_EDGE ( 'NONE', *, *, #14947, .F. ) ;
#13139 = EDGE_LOOP ( 'NONE', ( #4019, #19842, #11971, #17194 ) ) ;
#13140 = ORIENTED_EDGE ( 'NONE', *, *, #23354, .F. ) ;
#13141 = DIRECTION ( 'NONE',  ( -1.000000000000000000, -0.000000000000000000, -0.000000000000000000 ) ) ;
#13142 = CARTESIAN_POINT ( 'NONE',  ( 43.99999999999999289, -51.00000000000000711, 0.5000000000000000000 ) ) ;
#13143 = FACE_OUTER_BOUND ( 'NONE', #11873, .T. ) ;
#13144 = CARTESIAN_POINT ( 'NONE',  ( 5.871322893123448239, 8.081182679344781405, -5.506742014460233925 ) ) ;
#13145 = ORIENTED_EDGE ( 'NONE', *, *, #8354, .T. ) ;
#13146 = PRODUCT_DEFINITION_SHAPE ( 'NONE', 'NONE',  #24120 ) ;
#13147 = FACE_OUTER_BOUND ( 'NONE', #8783, .T. ) ;
#13148 = CARTESIAN_POINT ( 'NONE',  ( 23.00000000000000000, 1.102182119232617714E-15, -9.000000000000000000 ) ) ;
#13149 = CARTESIAN_POINT ( 'NONE',  ( 0.9999999999999986677, 0.000000000000000000, 0.000000000000000000 ) ) ;
#13150 = CARTESIAN_POINT ( 'NONE',  ( -28.99999999999999645, 29.50000000000000000, -3.000000000000000000 ) ) ;
#13151 = EDGE_CURVE ( 'NONE', #12121, #12921, #10602, .T. ) ;
#13152 = DIRECTION ( 'NONE',  ( -1.000000000000000000, -0.000000000000000000, -0.000000000000000000 ) ) ;
#13153 = ORIENTED_EDGE ( 'NONE', *, *, #5868, .T. ) ;
#13154 = CIRCLE ( 'NONE', #15101, 5.000000000000004441 ) ;
#13155 = EDGE_LOOP ( 'NONE', ( #15529, #10898, #13731, #18201 ) ) ;
#13156 = DIRECTION ( 'NONE',  ( -0.000000000000000000, -0.000000000000000000, -1.000000000000000000 ) ) ;
#13157 = VERTEX_POINT ( 'NONE', #16237 ) ;
#13158 = FACE_OUTER_BOUND ( 'NONE', #1964, .T. ) ;
#13159 = EDGE_CURVE ( 'NONE', #5970, #19012, #21661, .T. ) ;
#13160 = ADVANCED_FACE ( 'NONE', ( #5615 ), #127, .F. ) ;
#13161 = ORIENTED_EDGE ( 'NONE', *, *, #16064, .T. ) ;
#13162 =( LENGTH_UNIT ( ) NAMED_UNIT ( * ) SI_UNIT ( .MILLI., .METRE. ) );
#13163 = DIRECTION ( 'NONE',  ( 0.000000000000000000, 0.000000000000000000, 1.000000000000000000 ) ) ;
#13164 = FACE_OUTER_BOUND ( 'NONE', #24081, .T. ) ;
#13165 = DIRECTION ( 'NONE',  ( -1.000000000000000000, -0.000000000000000000, -0.000000000000000000 ) ) ;
#13166 = PLANE ( 'NONE',  #4112 ) ;
#13167 = VECTOR ( 'NONE', #1985, 1000.000000000000000 ) ;
#13168 = CARTESIAN_POINT ( 'NONE',  ( 0.000000000000000000, 0.000000000000000000, 0.000000000000000000 ) ) ;
#13169 = VECTOR ( 'NONE', #18103, 1000.000000000000000 ) ;
#13170 = CARTESIAN_POINT ( 'NONE',  ( 2.935661446562616295, -9.035036904803758873, -9.659589141758143427 ) ) ;
#13171 = ORIENTED_EDGE ( 'NONE', *, *, #22268, .T. ) ;
#13172 = DIRECTION ( 'NONE',  ( -1.000000000000000000, 0.000000000000000000, 0.000000000000000000 ) ) ;
#13173 = CARTESIAN_POINT ( 'NONE',  ( -6.822232771736904647E-13, 9.988891130263535700, 11.70674201446023410 ) ) ;
#13174 = ORIENTED_EDGE ( 'NONE', *, *, #23788, .F. ) ;
#13175 = CARTESIAN_POINT ( 'NONE',  ( 65.85249911436491743, -1.078520768856852078E-29, 5.000000000000007994 ) ) ;
#13176 = DIRECTION ( 'NONE',  ( -0.000000000000000000, -0.000000000000000000, -1.000000000000000000 ) ) ;
#13177 = CARTESIAN_POINT ( 'NONE',  ( 15.00000000000000178, 0.3242076166095267942, -9.499999999999987566 ) ) ;
#13178 = ADVANCED_FACE ( 'NONE', ( #7416 ), #480, .T. ) ;
#13179 = CARTESIAN_POINT ( 'NONE',  ( -1.831477161043247870, 8.813213971919513057, 78.61598362702075349 ) ) ;
#13180 = DIRECTION ( 'NONE',  ( -0.8757121056631641531, -0.4828336235133042775, 0.000000000000000000 ) ) ;
#13181 = DIRECTION ( 'NONE',  ( 0.000000000000000000, 0.000000000000000000, 1.000000000000000000 ) ) ;
#13182 = EDGE_CURVE ( 'NONE', #22169, #13221, #10717, .T. ) ;
#13183 = LINE ( 'NONE', #17088, #21958 ) ;
#13184 = ORIENTED_EDGE ( 'NONE', *, *, #15913, .F. ) ;
#13185 = FACE_OUTER_BOUND ( 'NONE', #1923, .T. ) ;
#13186 = FACE_OUTER_BOUND ( 'NONE', #22185, .T. ) ;
#13187 = ADVANCED_FACE ( 'NONE', ( #22461 ), #12670, .F. ) ;
#13188 = EDGE_CURVE ( 'NONE', #4993, #7176, #2309, .T. ) ;
#13189 = ADVANCED_FACE ( 'NONE', ( #11304 ), #8389, .T. ) ;
#13190 = DIRECTION ( 'NONE',  ( -0.000000000000000000, -0.000000000000000000, 1.000000000000000000 ) ) ;
#13191 = MECHANICAL_DESIGN_GEOMETRIC_PRESENTATION_REPRESENTATION (  '', ( #21406 ), #20062 ) ;
#13192 = CARTESIAN_POINT ( 'NONE',  ( 40.89823313241237912, 26.41789760203348081, -27.00000000000000000 ) ) ;
#13193 = APPLICATION_CONTEXT ( 'automotive_design' ) ;
#13194 = ORIENTED_EDGE ( 'NONE', *, *, #10962, .F. ) ;
#13195 = ORIENTED_EDGE ( 'NONE', *, *, #3676, .T. ) ;
#13196 = ORIENTED_EDGE ( 'NONE', *, *, #2494, .F. ) ;
#13197 = EDGE_LOOP ( 'NONE', ( #17485, #21769, #5654, #4099 ) ) ;
#13198 = LINE ( 'NONE', #1760, #1814 ) ;
#13199 = CARTESIAN_POINT ( 'NONE',  ( 29.00000000000000000, -29.50000000000000355, 11.50000000000000000 ) ) ;
#13200 = CIRCLE ( 'NONE', #2701, 15.00000000000000000 ) ;
#13201 = CARTESIAN_POINT ( 'NONE',  ( 9.000000000000000000, 0.000000000000000000, 15.00000000000000178 ) ) ;
#13202 = ORIENTED_EDGE ( 'NONE', *, *, #1536, .T. ) ;
#13203 = ORIENTED_EDGE ( 'NONE', *, *, #20421, .T. ) ;
#13204 = FACE_OUTER_BOUND ( 'NONE', #17975, .T. ) ;
#13205 = DIRECTION ( 'NONE',  ( -0.000000000000000000, -0.000000000000000000, -1.000000000000000000 ) ) ;
#13206 = ORIENTED_EDGE ( 'NONE', *, *, #22005, .T. ) ;
#13207 = EDGE_CURVE ( 'NONE', #530, #21660, #18772, .T. ) ;
#13208 = AXIS2_PLACEMENT_3D ( 'NONE', #12005, #10167, #8355 ) ;
#13209 = EDGE_LOOP ( 'NONE', ( #21797, #7666, #12135, #5568 ) ) ;
#13210 = DIRECTION ( 'NONE',  ( 0.000000000000000000, 0.000000000000000000, 1.000000000000000000 ) ) ;
#13211 = CARTESIAN_POINT ( 'NONE',  ( -5.976739099259236459E-13, 9.226949318570335734, -2.750781287208490689 ) ) ;
#13212 = DIRECTION ( 'NONE',  ( -1.000000000000000000, -1.224606353822377258E-16, -0.000000000000000000 ) ) ;
#13213 = EDGE_CURVE ( 'NONE', #10867, #1818, #2060, .T. ) ;
#13214 = DIRECTION ( 'NONE',  ( 0.000000000000000000, 0.000000000000000000, 1.000000000000000000 ) ) ;
#13215 = ORIENTED_EDGE ( 'NONE', *, *, #6558, .T. ) ;
#13216 = CARTESIAN_POINT ( 'NONE',  ( 11.50000000000000000, -14.80154252341788279, -10.02147513732838036 ) ) ;
#13217 = LINE ( 'NONE', #310, #17683 ) ;
#13218 = ORIENTED_EDGE ( 'NONE', *, *, #21020, .T. ) ;
#13219 = EDGE_CURVE ( 'NONE', #20932, #12170, #22046, .T. ) ;
#13220 = AXIS2_PLACEMENT_3D ( 'NONE', #6802, #1193, #1446 ) ;
#13221 = VERTEX_POINT ( 'NONE', #4155 ) ;
#13222 = CARTESIAN_POINT ( 'NONE',  ( 8.680847955711199049, -2.820578480813074496, 6.533165578109188409 ) ) ;
#13223 = ORIENTED_EDGE ( 'NONE', *, *, #18875, .F. ) ;
#13224 = SHAPE_DEFINITION_REPRESENTATION ( #20499, #2851 ) ;
#13225 = ORIENTED_EDGE ( 'NONE', *, *, #15525, .F. ) ;
#13226 = ORIENTED_EDGE ( 'NONE', *, *, #11566, .T. ) ;
#13227 = CARTESIAN_POINT ( 'NONE',  ( 64.39795365981944997, 7.562528597612068045E-15, 0.000000000000000000 ) ) ;
#13228 = CARTESIAN_POINT ( 'NONE',  ( -8.680847955711200825, 2.820578480813073607, -11.53316557810918574 ) ) ;
#13229 = DIRECTION ( 'NONE',  ( 0.000000000000000000, -1.000000000000000000, 0.000000000000000000 ) ) ;
#13230 = ORIENTED_EDGE ( 'NONE', *, *, #23850, .T. ) ;
#13231 = CARTESIAN_POINT ( 'NONE',  ( 20.64923905428956630, -37.45138642374539018, 11.00000000000000000 ) ) ;
#13232 = CARTESIAN_POINT ( 'NONE',  ( 0.000000000000000000, 0.000000000000000000, 12.50000000000000000 ) ) ;
#13233 = DIRECTION ( 'NONE',  ( -0.000000000000000000, -0.000000000000000000, -1.000000000000000000 ) ) ;
#13234 = DIRECTION ( 'NONE',  ( 0.000000000000000000, 0.000000000000000000, 1.000000000000000000 ) ) ;
#13235 = ORIENTED_EDGE ( 'NONE', *, *, #23856, .T. ) ;
#13236 = DIRECTION ( 'NONE',  ( 1.000000000000000000, 0.000000000000000000, 0.000000000000000000 ) ) ;
#13237 = AXIS2_PLACEMENT_3D ( 'NONE', #5486, #6967, #20151 ) ;
#13238 = EDGE_CURVE ( 'NONE', #18514, #8325, #20874, .T. ) ;
#13239 = ORIENTED_EDGE ( 'NONE', *, *, #10870, .T. ) ;
#13240 = DIRECTION ( 'NONE',  ( -1.000000000000000000, -1.224606353822377258E-16, -0.000000000000000000 ) ) ;
#13241 = LINE ( 'NONE', #20696, #1608 ) ;
#13242 = DIRECTION ( 'NONE',  ( 0.000000000000000000, -0.5000000000000011102, -0.8660254037844380415 ) ) ;
#13243 = DIRECTION ( 'NONE',  ( -0.7089874389501510388, 0.7052211081716897034, 0.000000000000000000 ) ) ;
#13244 = CARTESIAN_POINT ( 'NONE',  ( -5.871322893123449127, -8.081182679344781405, -5.359589141758143604 ) ) ;
#13245 = DIRECTION ( 'NONE',  ( 0.000000000000000000, 0.000000000000000000, 1.000000000000000000 ) ) ;
#13246 = EDGE_CURVE ( 'NONE', #19429, #4705, #6065, .T. ) ;
#13247 = ORIENTED_EDGE ( 'NONE', *, *, #13290, .F. ) ;
#13248 = EDGE_LOOP ( 'NONE', ( #14315, #4060, #9914, #11605, #20546, #10188 ) ) ;
#13249 = ORIENTED_EDGE ( 'NONE', *, *, #21566, .T. ) ;
#13250 = ORIENTED_EDGE ( 'NONE', *, *, #843, .F. ) ;
#13251 =( LENGTH_UNIT ( ) NAMED_UNIT ( * ) SI_UNIT ( .MILLI., .METRE. ) );
#13252 = AXIS2_PLACEMENT_3D ( 'NONE', #22369, #5769, #22493 ) ;
#13253 = ORIENTED_EDGE ( 'NONE', *, *, #5926, .T. ) ;
#13254 = CARTESIAN_POINT ( 'NONE',  ( 70.21613547800127719, -5.000000000000000000, 6.123233995736775157E-16 ) ) ;
#13255 = CARTESIAN_POINT ( 'NONE',  ( 0.000000000000000000, -7.812991839788663739, -16.07708877602020436 ) ) ;
#13256 = UNCERTAINTY_MEASURE_WITH_UNIT (LENGTH_MEASURE( 1.000000000000000082E-05 ), #21358, 'distance_accuracy_value', 'NONE');
#13257 = DIRECTION ( 'NONE',  ( -1.000000000000000000, 0.000000000000000000, 0.000000000000000000 ) ) ;
#13258 = CARTESIAN_POINT ( 'NONE',  ( 66.14750088563508257, -5.000000000000009770, 0.000000000000000000 ) ) ;
#13259 = SURFACE_STYLE_USAGE ( .BOTH. , #11289 ) ;
#13260 = CARTESIAN_POINT ( 'NONE',  ( -9.500000000000202505, 3.086737114211975275, -6.106742014460232681 ) ) ;
#13261 = ADVANCED_FACE ( 'NONE', ( #9615 ), #12290, .T. ) ;
#13262 = CARTESIAN_POINT ( 'NONE',  ( -14.99999999999999822, 6.045577542124163753E-21, -9.499999999999994671 ) ) ;
#13263 = EDGE_CURVE ( 'NONE', #7176, #10867, #11567, .T. ) ;
#13264 = CARTESIAN_POINT ( 'NONE',  ( -20.85000000000000497, 15.03999999999999915, 2.200000000000000178 ) ) ;
#13265 = DIRECTION ( 'NONE',  ( 1.000000000000000000, 0.000000000000000000, 0.000000000000000000 ) ) ;
#13266 = DIRECTION ( 'NONE',  ( 1.000000000000000000, 0.000000000000000000, 0.000000000000000000 ) ) ;
#13267 = FACE_OUTER_BOUND ( 'NONE', #8609, .T. ) ;
#13268 = TOROIDAL_SURFACE ( 'NONE', #19530, 5.999999999999999112, 1.000000000000000000 ) ;
#13269 = CARTESIAN_POINT ( 'NONE',  ( 0.000000000000000000, 0.000000000000000000, 6.000000000000000000 ) ) ;
#13270 = PRODUCT_DEFINITION_SHAPE ( 'NONE', 'NONE',  #12542 ) ;
#13271 = ORIENTED_EDGE ( 'NONE', *, *, #993, .T. ) ;
#13272 = AXIS2_PLACEMENT_3D ( 'NONE', #12492, #6430, #12383 ) ;
#13273 = CARTESIAN_POINT ( 'NONE',  ( -1.999999999999996669, 45.00000000000000000, -8.673617379884035472E-16 ) ) ;
#13274 = VERTEX_POINT ( 'NONE', #7472 ) ;
#13275 = DIRECTION ( 'NONE',  ( -1.000000000000000000, 0.000000000000000000, 0.000000000000000000 ) ) ;
#13276 = VERTEX_POINT ( 'NONE', #22400 ) ;
#13277 = CARTESIAN_POINT ( 'NONE',  ( -2.935661446562617183, 9.035036904803758873, 8.659589141758143427 ) ) ;
#13278 = EDGE_LOOP ( 'NONE', ( #21950, #22459, #21777, #17927 ) ) ;
#13279 = SHAPE_REPRESENTATION_RELATIONSHIP ( 'NONE' , 'NONE' ,  #6130, #3483 ) ;
#13280 = LINE ( 'NONE', #20736, #23877 ) ;
#13281 = FACE_OUTER_BOUND ( 'NONE', #1830, .T. ) ;
#13282 = DIRECTION ( 'NONE',  ( 0.000000000000000000, 0.000000000000000000, 1.000000000000000000 ) ) ;
#13283 = FACE_OUTER_BOUND ( 'NONE', #9014, .T. ) ;
#13284 = AXIS2_PLACEMENT_3D ( 'NONE', #14738, #12424, #3284 ) ;
#13285 = VECTOR ( 'NONE', #4974, 1000.000000000000000 ) ;
#13286 = CARTESIAN_POINT ( 'NONE',  ( 7.685661446562381371, -5.583959896777971110, -9.859589141758144493 ) ) ;
#13287 = ORIENTED_EDGE ( 'NONE', *, *, #6889, .T. ) ;
#13288 = CARTESIAN_POINT ( 'NONE',  ( -9.500000000000000000, -6.482511860946779655E-13, 8.206742014460234103 ) ) ;
#13289 = EDGE_CURVE ( 'NONE', #11455, #15083, #21273, .T. ) ;
#13290 = EDGE_CURVE ( 'NONE', #18576, #17720, #9558, .T. ) ;
#13291 = VERTEX_POINT ( 'NONE', #20207 ) ;
#13292 = LINE ( 'NONE', #7558, #10625 ) ;
#13293 = CARTESIAN_POINT ( 'NONE',  ( 3.000000000000000888, 8.485281374238567764, 80.80016882425942981 ) ) ;
#13294 = DIRECTION ( 'NONE',  ( -1.000000000000000000, -0.000000000000000000, 0.000000000000000000 ) ) ;
#13295 = DIRECTION ( 'NONE',  ( -1.000000000000000000, 0.000000000000000000, 0.000000000000000000 ) ) ;
#13296 = CARTESIAN_POINT ( 'NONE',  ( -0.9705301899670187860, 8.949407723703927786, 78.15445800498790163 ) ) ;
#13297 = CARTESIAN_POINT ( 'NONE',  ( 7.685661446561619314, 5.583959896779020049, -7.406742014460233392 ) ) ;
#13298 = LINE ( 'NONE', #7230, #11401 ) ;
#13299 = AXIS2_PLACEMENT_3D ( 'NONE', #18766, #249, #7529 ) ;
#13300 = VERTEX_POINT ( 'NONE', #11013 ) ;
#13301 = CARTESIAN_POINT ( 'NONE',  ( -28.73477696352899002, 42.73830357953206516, 0.000000000000000000 ) ) ;
#13302 = FACE_OUTER_BOUND ( 'NONE', #8883, .T. ) ;
#13303 = FACE_OUTER_BOUND ( 'NONE', #16594, .T. ) ;
#13304 = AXIS2_PLACEMENT_3D ( 'NONE', #9303, #23746, #14439 ) ;
#13305 = LINE ( 'NONE', #7693, #24029 ) ;
#13306 = CARTESIAN_POINT ( 'NONE',  ( -39.99999999999999289, -27.79189783386527779, 27.00000000000000000 ) ) ;
#13307 = EDGE_LOOP ( 'NONE', ( #14393, #14446, #14040, #13063 ) ) ;
#13308 = PRODUCT_DEFINITION ( 'UNKNOWN', '', #12318, #20922 ) ;
#13309 = ADVANCED_FACE ( 'NONE', ( #18487 ), #18160, .T. ) ;
#13310 = EDGE_LOOP ( 'NONE', ( #3878, #9482, #3568, #2760, #674 ) ) ;
#13311 = ITEM_DEFINED_TRANSFORMATION ( 'NONE', 'NONE', #24014,  #8005 ) ;
#13312 = VERTEX_POINT ( 'NONE', #7262 ) ;
#13313 = CYLINDRICAL_SURFACE ( 'NONE', #2946, 14.99999999999999822 ) ;
#13314 = EDGE_CURVE ( 'NONE', #12468, #9726, #3842, .T. ) ;
#13315 = LINE ( 'NONE', #13201, #5575 ) ;
#13316 = ORIENTED_EDGE ( 'NONE', *, *, #10265, .T. ) ;
#13317 = AXIS2_PLACEMENT_3D ( 'NONE', #3977, #11396, #11530 ) ;
#13318 = ORIENTED_EDGE ( 'NONE', *, *, #13159, .T. ) ;
#13319 = AXIS2_PLACEMENT_3D ( 'NONE', #19665, #10370, #23439 ) ;
#13320 = EDGE_CURVE ( 'NONE', #1690, #13078, #5681, .T. ) ;
#13321 = AXIS2_PLACEMENT_3D ( 'NONE', #21859, #12695, #10615 ) ;
#13322 = CIRCLE ( 'NONE', #9042, 8.000000000000003553 ) ;
#13323 = EDGE_CURVE ( 'NONE', #1117, #19378, #18720, .T. ) ;
#13324 = CYLINDRICAL_SURFACE ( 'NONE', #18648, 8.999999999999994671 ) ;
#13325 = CIRCLE ( 'NONE', #23475, 4.172000000000008590 ) ;
#13326 = VERTEX_POINT ( 'NONE', #5434 ) ;
#13327 = CARTESIAN_POINT ( 'NONE',  ( -4.327215458830174555, -8.475258530630579656, -3.501890472894100714 ) ) ;
#13328 = VECTOR ( 'NONE', #6146, 1000.000000000000000 ) ;
#13329 = AXIS2_PLACEMENT_3D ( 'NONE', #9524, #9173, #16975 ) ;
#13330 = VERTEX_POINT ( 'NONE', #12979 ) ;
#13331 = CARTESIAN_POINT ( 'NONE',  ( 3.890962118697714531E-15, 15.50000000000000000, 7.699999999999998401 ) ) ;
#13332 = DIRECTION ( 'NONE',  ( -0.000000000000000000, 0.000000000000000000, 1.000000000000000000 ) ) ;
#13333 = DIRECTION ( 'NONE',  ( -1.000000000000000000, -0.000000000000000000, -0.000000000000000000 ) ) ;
#13334 = PRODUCT_DEFINITION_CONTEXT ( 'detailed design', #21014, 'design' ) ;
#13335 = CARTESIAN_POINT ( 'NONE',  ( 1.224646799147352714E-16, -14.99147757894464306, 8.749999999999998224 ) ) ;
#13336 = ORIENTED_EDGE ( 'NONE', *, *, #5250, .T. ) ;
#13337 = CARTESIAN_POINT ( 'NONE',  ( -41.00000000000000000, -5.000000000000000888, 11.00000000000000000 ) ) ;
#13338 = CARTESIAN_POINT ( 'NONE',  ( 0.000000000000000000, 0.000000000000000000, 3.499999999999999556 ) ) ;
#13339 = VERTEX_POINT ( 'NONE', #7366 ) ;
#13340 = ORIENTED_EDGE ( 'NONE', *, *, #688, .T. ) ;
#13341 = CARTESIAN_POINT ( 'NONE',  ( -2.682529543900285862, 8.255977015246234174, 5.233165578109188587 ) ) ;
#13342 = ORIENTED_EDGE ( 'NONE', *, *, #12367, .F. ) ;
#13343 = AXIS2_PLACEMENT_3D ( 'NONE', #5474, #19779, #6952 ) ;
#13344 = CIRCLE ( 'NONE', #1675, 5.000000000000007994 ) ;
#13345 = AXIS2_PLACEMENT_3D ( 'NONE', #5889, #409, #13458 ) ;
#13346 = AXIS2_PLACEMENT_3D ( 'NONE', #23134, #3885, #2177 ) ;
#13347 = DIRECTION ( 'NONE',  ( 0.000000000000000000, 0.000000000000000000, -1.000000000000000000 ) ) ;
#13348 = EDGE_CURVE ( 'NONE', #19800, #3126, #20315, .T. ) ;
#13349 = AXIS2_PLACEMENT_3D ( 'NONE', #13431, #384, #19166 ) ;
#13350 = ORIENTED_EDGE ( 'NONE', *, *, #3675, .F. ) ;
#13351 = ORIENTED_EDGE ( 'NONE', *, *, #12163, .F. ) ;
#13352 = PRODUCT_DEFINITION_SHAPE ( 'NONE', 'NONE',  #24119 ) ;
#13353 = DIRECTION ( 'NONE',  ( -1.000000000000000000, -0.000000000000000000, -0.000000000000000000 ) ) ;
#13354 = CARTESIAN_POINT ( 'NONE',  ( -5.871322893124554021, 8.081182679343978492, -2.759589141758142627 ) ) ;
#13355 = VECTOR ( 'NONE', #2630, 1000.000000000000000 ) ;
#13356 = DIRECTION ( 'NONE',  ( -1.000000000000000000, 2.600433232233976523E-16, -0.000000000000000000 ) ) ;
#13357 = VERTEX_POINT ( 'NONE', #5190 ) ;
#13358 = DIRECTION ( 'NONE',  ( -1.000000000000000000, 0.000000000000000000, 0.000000000000000000 ) ) ;
#13359 = PLANE ( 'NONE',  #11924 ) ;
#13360 = LINE ( 'NONE', #9934, #7819 ) ;
#13361 = EDGE_CURVE ( 'NONE', #4017, #4495, #22162, .T. ) ;
#13362 = DIRECTION ( 'NONE',  ( -0.000000000000000000, -0.000000000000000000, 1.000000000000000000 ) ) ;
#13363 = EDGE_CURVE ( 'NONE', #4173, #19649, #14806, .T. ) ;
#13364 = CARTESIAN_POINT ( 'NONE',  ( 29.00000000000000711, -29.50000000000000711, 27.00000000000000000 ) ) ;
#13365 = CARTESIAN_POINT ( 'NONE',  ( 31.10231664966676846, -45.36128193761570770, 0.000000000000000000 ) ) ;
#13366 = DIRECTION ( 'NONE',  ( -1.000000000000000000, -0.000000000000000000, -0.000000000000000000 ) ) ;
#13367 = AXIS2_PLACEMENT_3D ( 'NONE', #5000, #10916, #10810 ) ;
#13368 = ORIENTED_EDGE ( 'NONE', *, *, #12830, .T. ) ;
#13369 = DIRECTION ( 'NONE',  ( -0.000000000000000000, -0.000000000000000000, -1.000000000000000000 ) ) ;
#13370 = DIRECTION ( 'NONE',  ( -1.000000000000000000, 0.000000000000000000, 0.000000000000000000 ) ) ;
#13371 = CIRCLE ( 'NONE', #15704, 5.000000000000007994 ) ;
#13372 = CARTESIAN_POINT ( 'NONE',  ( 41.73082370883258818, -27.62204025492844650, -1.500000000000000000 ) ) ;
#13373 = DIRECTION ( 'NONE',  ( -0.000000000000000000, 1.000000000000000000, -0.000000000000000000 ) ) ;
#13374 = AXIS2_PLACEMENT_3D ( 'NONE', #10784, #3241, #10670 ) ;
#13375 = ADVANCED_BREP_SHAPE_REPRESENTATION ( '', ( #2970, #8005 ), #7613 ) ;
#13376 = AXIS2_PLACEMENT_3D ( 'NONE', #22879, #784, #4584 ) ;
#13377 = CYLINDRICAL_SURFACE ( 'NONE', #17723, 1.000000000000000888 ) ;
#13378 = DIRECTION ( 'NONE',  ( -1.000000000000000000, 0.000000000000000000, 0.000000000000000000 ) ) ;
#13379 = VECTOR ( 'NONE', #2042, 1000.000000000000000 ) ;
#13380 = ORIENTED_EDGE ( 'NONE', *, *, #12074, .T. ) ;
#13381 = EDGE_LOOP ( 'NONE', ( #15025, #9350, #7139, #2019 ) ) ;
#13382 = APPLICATION_CONTEXT ( 'automotive_design' ) ;
#13383 = EDGE_LOOP ( 'NONE', ( #12868, #23360, #10787, #6832 ) ) ;
#13384 = VECTOR ( 'NONE', #4780, 1000.000000000000000 ) ;
#13385 = VERTEX_POINT ( 'NONE', #3366 ) ;
#13386 = FACE_OUTER_BOUND ( 'NONE', #15286, .T. ) ;
#13387 = VECTOR ( 'NONE', #783, 999.9999999999998863 ) ;
#13388 = CIRCLE ( 'NONE', #5994, 1.499999999999999778 ) ;
#13389 = DIRECTION ( 'NONE',  ( -1.000000000000000000, 5.501724186093585079E-16, 0.000000000000000000 ) ) ;
#13390 = CARTESIAN_POINT ( 'NONE',  ( 75.45454545454545325, 7.491529369508391930E-15, 0.000000000000000000 ) ) ;
#13391 = DIRECTION ( 'NONE',  ( 1.000000000000000000, 0.000000000000000000, 0.000000000000000000 ) ) ;
#13392 = DIRECTION ( 'NONE',  ( -1.000000000000000000, 0.000000000000000000, 0.000000000000000000 ) ) ;
#13393 = AXIS2_PLACEMENT_3D ( 'NONE', #6292, #13738, #4976 ) ;
#13394 = ADVANCED_FACE ( 'NONE', ( #12856 ), #18254, .T. ) ;
#13395 = CIRCLE ( 'NONE', #9474, 4.172000000000008590 ) ;
#13396 = DIRECTION ( 'NONE',  ( 0.000000000000000000, -1.000000000000000000, 0.000000000000000000 ) ) ;
#13397 = ORIENTED_EDGE ( 'NONE', *, *, #12571, .T. ) ;
#13398 = CONICAL_SURFACE ( 'NONE', #1727, 7.999999999999986677, 0.7853981633974473908 ) ;
#13399 = DIRECTION ( 'NONE',  ( 1.000000000000000000, 1.224606353822377258E-16, 0.000000000000000000 ) ) ;
#13400 = CARTESIAN_POINT ( 'NONE',  ( -20.85000000000000853, 15.04000000000000092, -25.00000000000000000 ) ) ;
#13401 = DIRECTION ( 'NONE',  ( -1.000000000000000000, -0.000000000000000000, -0.000000000000000000 ) ) ;
#13402 = EDGE_LOOP ( 'NONE', ( #8404, #9271, #13046, #11868, #22068 ) ) ;
#13403 = DIRECTION ( 'NONE',  ( 0.000000000000000000, 0.000000000000000000, 1.000000000000000000 ) ) ;
#13404 = CIRCLE ( 'NONE', #2902, 1.999999999999994449 ) ;
#13405 = VERTEX_POINT ( 'NONE', #1777 ) ;
#13406 = VECTOR ( 'NONE', #4186, 1000.000000000000000 ) ;
#13407 = VERTEX_POINT ( 'NONE', #23751 ) ;
#13408 = CARTESIAN_POINT ( 'NONE',  ( -5.871322893124554021, 8.081182679343978492, 8.759589141758141295 ) ) ;
#13409 = EDGE_CURVE ( 'NONE', #9227, #5616, #16250, .T. ) ;
#13410 = CONICAL_SURFACE ( 'NONE', #10672, 9.000000000000000000, 0.7853981633974482790 ) ;
#13411 = ORIENTED_EDGE ( 'NONE', *, *, #659, .T. ) ;
#13412 = DIRECTION ( 'NONE',  ( 1.000000000000000000, 0.000000000000000000, 0.000000000000000000 ) ) ;
#13413 = CARTESIAN_POINT ( 'NONE',  ( 27.70933665152130487, -40.41277845351217479, 11.00000000000000000 ) ) ;
#13414 = DIRECTION ( 'NONE',  ( -1.000000000000000000, 3.469446951953611033E-15, 0.000000000000000000 ) ) ;
#13415 = AXIS2_PLACEMENT_3D ( 'NONE', #8253, #3039, #16202 ) ;
#13416 = DIRECTION ( 'NONE',  ( -1.000000000000000000, 0.000000000000000000, 0.000000000000000000 ) ) ;
#13417 = EDGE_CURVE ( 'NONE', #13748, #1974, #20433, .T. ) ;
#13418 = DIRECTION ( 'NONE',  ( 0.000000000000000000, -1.000000000000000000, 0.000000000000000000 ) ) ;
#13419 = EDGE_CURVE ( 'NONE', #2676, #18226, #22044, .T. ) ;
#13420 = CARTESIAN_POINT ( 'NONE',  ( 14.94777716362147935, -1.291632522116889170, -9.417361603030268924 ) ) ;
#13421 = EDGE_CURVE ( 'NONE', #8124, #9276, #12746, .T. ) ;
#13422 = DIRECTION ( 'NONE',  ( -1.000000000000000000, 0.000000000000000000, 0.000000000000000000 ) ) ;
#13423 = AXIS2_PLACEMENT_3D ( 'NONE', #6636, #17862, #21402 ) ;
#13424 = CARTESIAN_POINT ( 'NONE',  ( 9.500000000000209610, -3.086737114211962396, -3.959589141758145026 ) ) ;
#13425 = ORIENTED_EDGE ( 'NONE', *, *, #18905, .F. ) ;
#13426 = AXIS2_PLACEMENT_3D ( 'NONE', #22395, #1890, #22746 ) ;
#13427 = DIRECTION ( 'NONE',  ( 1.000000000000000000, 0.000000000000000000, 0.000000000000000000 ) ) ;
#13428 = VERTEX_POINT ( 'NONE', #4325 ) ;
#13429 = CARTESIAN_POINT ( 'NONE',  ( -31.74999999999995737, 0.000000000000000000, 5.000000000000000888 ) ) ;
#13430 = AXIS2_PLACEMENT_3D ( 'NONE', #2780, #146, #22481 ) ;
#13431 = CARTESIAN_POINT ( 'NONE',  ( 60.03431729618309021, 7.562528597612068045E-15, 0.000000000000000000 ) ) ;
#13432 = FACE_OUTER_BOUND ( 'NONE', #1142, .T. ) ;
#13433 = AXIS2_PLACEMENT_3D ( 'NONE', #16935, #17302, #3889 ) ;
#13434 = DIRECTION ( 'NONE',  ( 0.000000000000000000, 1.000000000000000000, 0.000000000000000000 ) ) ;
#13435 = DIRECTION ( 'NONE',  ( 0.000000000000000000, 0.000000000000000000, 1.000000000000000000 ) ) ;
#13436 = DIRECTION ( 'NONE',  ( 0.000000000000000000, 0.000000000000000000, 1.000000000000000000 ) ) ;
#13437 = DIRECTION ( 'NONE',  ( -1.000000000000000000, -0.000000000000000000, -0.000000000000000000 ) ) ;
#13438 = AXIS2_PLACEMENT_3D ( 'NONE', #3879, #18537, #14739 ) ;
#13439 = MECHANICAL_DESIGN_GEOMETRIC_PRESENTATION_REPRESENTATION (  '', ( #1007 ), #19700 ) ;
#13440 = DIRECTION ( 'NONE',  ( -0.000000000000000000, -0.000000000000000000, -1.000000000000000000 ) ) ;
#13441 = VERTEX_POINT ( 'NONE', #3954 ) ;
#13442 = DIRECTION ( 'NONE',  ( -1.000000000000000000, 0.000000000000000000, 0.000000000000000000 ) ) ;
#13443 = CARTESIAN_POINT ( 'NONE',  ( -2.682529543899159208, -8.255977015246598327, 12.03316557810918930 ) ) ;
#13444 = CARTESIAN_POINT ( 'NONE',  ( 70.51113724927145654, -4.999999999999989342, 0.000000000000000000 ) ) ;
#13445 = CARTESIAN_POINT ( 'NONE',  ( 2.024999999999999911, -45.00000000000000000, 27.00000000000000000 ) ) ;
#13446 = ADVANCED_FACE ( 'NONE', ( #22883 ), #311, .F. ) ;
#13447 = EDGE_CURVE ( 'NONE', #13479, #11063, #23234, .T. ) ;
#13448 = ORIENTED_EDGE ( 'NONE', *, *, #21367, .T. ) ;
#13449 = AXIS2_PLACEMENT_3D ( 'NONE', #5303, #15139, #11340 ) ;
#13450 = AXIS2_PLACEMENT_3D ( 'NONE', #14402, #12813, #8801 ) ;
#13451 = VERTEX_POINT ( 'NONE', #22624 ) ;
#13452 = LINE ( 'NONE', #10131, #20477 ) ;
#13453 = VECTOR ( 'NONE', #15592, 1000.000000000000114 ) ;
#13454 = VECTOR ( 'NONE', #18075, 1000.000000000000000 ) ;
#13455 = CARTESIAN_POINT ( 'NONE',  ( -6.822232771736903637E-13, 9.988891130263535700, -9.706742014460232326 ) ) ;
#13456 = ORIENTED_EDGE ( 'NONE', *, *, #1350, .F. ) ;
#13457 = EDGE_LOOP ( 'NONE', ( #20569, #21757, #13826, #12654 ) ) ;
#13458 = DIRECTION ( 'NONE',  ( 0.000000000000000000, 0.000000000000000000, 1.000000000000000000 ) ) ;
#13459 = CARTESIAN_POINT ( 'NONE',  ( 0.000000000000000000, -45.00000000000000000, 0.000000000000000000 ) ) ;
#13460 = ORIENTED_EDGE ( 'NONE', *, *, #15086, .F. ) ;
#13461 = CARTESIAN_POINT ( 'NONE',  ( -47.34180362313354351, -5.000000000000002665, 10.49999999999999822 ) ) ;
#13462 = EDGE_LOOP ( 'NONE', ( #6268, #16711, #7992, #9430 ) ) ;
#13463 = CARTESIAN_POINT ( 'NONE',  ( 30.31394790604173295, -39.41330121100981643, 12.00000000000000000 ) ) ;
#13464 = FACE_BOUND ( 'NONE', #3910, .T. ) ;
#13465 = SPHERICAL_SURFACE ( 'NONE', #7881, 1.000000000000000000 ) ;
#13466 = AXIS2_PLACEMENT_3D ( 'NONE', #14617, #23550, #18292 ) ;
#13467 = ADVANCED_FACE ( 'NONE', ( #19208 ), #18977, .F. ) ;
#13468 = CIRCLE ( 'NONE', #5698, 1.000000000000000888 ) ;
#13469 = CARTESIAN_POINT ( 'NONE',  ( -2.024999999999999911, -45.00000000000000000, 27.00000000000000000 ) ) ;
#13470 = ORIENTED_EDGE ( 'NONE', *, *, #15832, .T. ) ;
#13471 = CARTESIAN_POINT ( 'NONE',  ( -30.44534269664590553, 40.40463133211079594, 12.00000000000000000 ) ) ;
#13472 = CARTESIAN_POINT ( 'NONE',  ( 10.40000000000000036, 0.000000000000000000, 0.000000000000000000 ) ) ;
#13473 = CARTESIAN_POINT ( 'NONE',  ( 23.00000000000000000, 11.37860023611358962, -13.78561139983841421 ) ) ;
#13474 = VERTEX_POINT ( 'NONE', #9669 ) ;
#13475 = AXIS2_PLACEMENT_3D ( 'NONE', #23630, #20195, #22155 ) ;
#13476 = EDGE_CURVE ( 'NONE', #15214, #3956, #8791, .T. ) ;
#13477 = ORIENTED_EDGE ( 'NONE', *, *, #10422, .F. ) ;
#13478 = CARTESIAN_POINT ( 'NONE',  ( -5.871322893123450015, -8.081182679344781405, 11.35958914175814272 ) ) ;
#13479 = VERTEX_POINT ( 'NONE', #13473 ) ;
#13480 = ADVANCED_FACE ( 'NONE', ( #15274 ), #20929, .T. ) ;
#13481 = ORIENTED_EDGE ( 'NONE', *, *, #12997, .T. ) ;
#13482 = EDGE_CURVE ( 'NONE', #22724, #12105, #2587, .T. ) ;
#13483 = CYLINDRICAL_SURFACE ( 'NONE', #20853, 5.099999999999996980 ) ;
#13484 = VERTEX_POINT ( 'NONE', #19827 ) ;
#13485 = VERTEX_POINT ( 'NONE', #19455 ) ;
#13486 = CARTESIAN_POINT ( 'NONE',  ( 83.30704456891035647, 7.562528597612068045E-15, 0.000000000000000000 ) ) ;
#13487 = DIRECTION ( 'NONE',  ( -1.000000000000000000, -1.224606353822377258E-16, -0.000000000000000000 ) ) ;
#13488 = AXIS2_PLACEMENT_3D ( 'NONE', #829, #12026, #4371 ) ;
#13489 = AXIS2_PLACEMENT_3D ( 'NONE', #2532, #9950, #22918 ) ;
#13490 = DIRECTION ( 'NONE',  ( 0.000000000000000000, -1.000000000000000000, 0.000000000000000000 ) ) ;
#13491 = CIRCLE ( 'NONE', #5718, 9.725923461386809521 ) ;
#13492 = VERTEX_POINT ( 'NONE', #8576 ) ;
#13493 = CYLINDRICAL_SURFACE ( 'NONE', #16153, 1.000000000000002442 ) ;
#13494 = FACE_OUTER_BOUND ( 'NONE', #4860, .T. ) ;
#13495 = CARTESIAN_POINT ( 'NONE',  ( 1.500000000000001332, 0.000000000000000000, 8.000000000000000000 ) ) ;
#13496 = DIRECTION ( 'NONE',  ( -0.000000000000000000, -0.000000000000000000, 1.000000000000000000 ) ) ;
#13497 = EDGE_LOOP ( 'NONE', ( #16467, #8516 ) ) ;
#13498 = CYLINDRICAL_SURFACE ( 'NONE', #235, 4.249999999999996447 ) ;
#13499 = CONICAL_SURFACE ( 'NONE', #21294, 4.172000000000008590, 0.9599310885968742602 ) ;
#13500 = DIRECTION ( 'NONE',  ( -1.000000000000000000, -0.000000000000000000, -0.000000000000000000 ) ) ;
#13501 = ORIENTED_EDGE ( 'NONE', *, *, #21566, .F. ) ;
#13502 = CARTESIAN_POINT ( 'NONE',  ( -30.44534269664590198, 40.40463133211079594, 27.00000000000000000 ) ) ;
#13503 = LINE ( 'NONE', #3978, #1236 ) ;
#13504 = CARTESIAN_POINT ( 'NONE',  ( -23.85000000000000497, 15.03999999999999915, 25.00000000000000000 ) ) ;
#13505 = EDGE_CURVE ( 'NONE', #1599, #9132, #17871, .T. ) ;
#13506 = CARTESIAN_POINT ( 'NONE',  ( -1.999999999999994449, -45.00000000000000000, 23.99999999999999645 ) ) ;
#13507 = DIRECTION ( 'NONE',  ( -1.000000000000000000, 0.000000000000000000, 0.000000000000000000 ) ) ;
#13508 = AXIS2_PLACEMENT_3D ( 'NONE', #17622, #13863, #21310 ) ;
#13509 = CARTESIAN_POINT ( 'NONE',  ( 9.500000000000000000, 6.470877716354879437E-13, 9.206742014460234103 ) ) ;
#13510 = AXIS2_PLACEMENT_3D ( 'NONE', #7245, #20551, #9535 ) ;
#13511 = ORIENTED_EDGE ( 'NONE', *, *, #139, .T. ) ;
#13512 = CARTESIAN_POINT ( 'NONE',  ( -7.022953521754877748, -5.102474405760673015, 9.833165578109188232 ) ) ;
#13513 = ADVANCED_FACE ( 'NONE', ( #17604 ), #2733, .T. ) ;
#13514 = ADVANCED_FACE ( 'NONE', ( #8693 ), #7602, .T. ) ;
#13515 = ORIENTED_EDGE ( 'NONE', *, *, #12367, .T. ) ;
#13516 = DIRECTION ( 'NONE',  ( 0.0006440730211827849078, -0.9999997925849501978, -6.843601108204850534E-17 ) ) ;
#13517 = AXIS2_PLACEMENT_3D ( 'NONE', #1578, #1349, #19887 ) ;
#13518 = CARTESIAN_POINT ( 'NONE',  ( 70.51113724927145654, 7.420530141404717394E-15, 0.000000000000000000 ) ) ;
#13519 = ORIENTED_EDGE ( 'NONE', *, *, #20655, .F. ) ;
#13520 = CARTESIAN_POINT ( 'NONE',  ( -31.74999999999995737, 0.000000000000000000, 0.000000000000000000 ) ) ;
#13521 = DIRECTION ( 'NONE',  ( -1.000000000000000000, -0.000000000000000000, -0.000000000000000000 ) ) ;
#13522 = UNCERTAINTY_MEASURE_WITH_UNIT (LENGTH_MEASURE( 1.000000000000000082E-05 ), #20478, 'distance_accuracy_value', 'NONE');
#13523 = DIRECTION ( 'NONE',  ( -0.000000000000000000, 0.000000000000000000, -1.000000000000000000 ) ) ;
#13524 = CARTESIAN_POINT ( 'NONE',  ( 40.66734255040738333, 26.56420859267091217, -1.500000000000000000 ) ) ;
#13525 = CARTESIAN_POINT ( 'NONE',  ( -7.685661446561619314, -5.583959896779019161, 6.406742014460233392 ) ) ;
#13526 = EDGE_LOOP ( 'NONE', ( #14181, #2909, #14659 ) ) ;
#13527 = AXIS2_PLACEMENT_3D ( 'NONE', #13390, #20855, #4137 ) ;
#13528 = CARTESIAN_POINT ( 'NONE',  ( 0.000000000000000000, 0.000000000000000000, 0.000000000000000000 ) ) ;
#13529 = LINE ( 'NONE', #20972, #3327 ) ;
#13530 = ORIENTED_EDGE ( 'NONE', *, *, #23641, .T. ) ;
#13531 = DIRECTION ( 'NONE',  ( -1.000000000000000000, -1.224606353822377258E-16, -0.000000000000000000 ) ) ;
#13532 = FACE_OUTER_BOUND ( 'NONE', #10306, .T. ) ;
#13533 = CARTESIAN_POINT ( 'NONE',  ( 0.000000000000000000, 15.03999999999999915, -25.00000000000000000 ) ) ;
#13534 = EDGE_CURVE ( 'NONE', #22152, #2457, #11985, .T. ) ;
#13535 = CARTESIAN_POINT ( 'NONE',  ( 35.99999999999992184, 59.99999999999998579, 0.000000000000000000 ) ) ;
#13536 = ORIENTED_EDGE ( 'NONE', *, *, #2463, .F. ) ;
#13537 = ORIENTED_EDGE ( 'NONE', *, *, #21127, .F. ) ;
#13538 = EDGE_LOOP ( 'NONE', ( #15630, #19818, #4748, #1476 ) ) ;
#13539 = CARTESIAN_POINT ( 'NONE',  ( 6.809999908187194197E-13, -9.988891130263535700, 9.559589141758145558 ) ) ;
#13540 = DIRECTION ( 'NONE',  ( -1.000000000000000000, 0.000000000000000000, 0.000000000000000000 ) ) ;
#13541 = DIRECTION ( 'NONE',  ( 0.000000000000000000, -0.000000000000000000, -1.000000000000000000 ) ) ;
#13542 = EDGE_CURVE ( 'NONE', #19938, #14137, #4718, .T. ) ;
#13543 = VERTEX_POINT ( 'NONE', #23612 ) ;
#13544 =( LENGTH_UNIT ( ) NAMED_UNIT ( * ) SI_UNIT ( .MILLI., .METRE. ) );
#13545 = DIRECTION ( 'NONE',  ( 0.000000000000000000, -4.625929269271485322E-15, -1.000000000000000000 ) ) ;
#13546 = FACE_OUTER_BOUND ( 'NONE', #11265, .T. ) ;
#13547 = LINE ( 'NONE', #8149, #17811 ) ;
#13548 = VERTEX_POINT ( 'NONE', #8468 ) ;
#13549 = DIRECTION ( 'NONE',  ( 0.000000000000000000, 0.000000000000000000, -1.000000000000000000 ) ) ;
#13550 = CARTESIAN_POINT ( 'NONE',  ( 0.000000000000000000, 8.878689293818310074E-16, -6.500000000000000888 ) ) ;
#13551 = LINE ( 'NONE', #11686, #6322 ) ;
#13552 = CARTESIAN_POINT ( 'NONE',  ( 11.50000000000000000, 2.119223430970397892, -17.74893002550478016 ) ) ;
#13553 = ORIENTED_EDGE ( 'NONE', *, *, #15735, .T. ) ;
#13554 = FACE_OUTER_BOUND ( 'NONE', #10017, .T. ) ;
#13555 = EDGE_CURVE ( 'NONE', #11452, #15990, #1161, .T. ) ;
#13556 = CARTESIAN_POINT ( 'NONE',  ( -4.622819170558153168, -7.943728616300125722, 12.31730142689806051 ) ) ;
#13557 = AXIS2_PLACEMENT_3D ( 'NONE', #5450, #9221, #8967 ) ;
#13558 = CARTESIAN_POINT ( 'NONE',  ( 0.7812760552145768811, 8.968134317516772924, 78.09676514898454514 ) ) ;
#13559 = CIRCLE ( 'NONE', #21755, 5.000000000000007994 ) ;
#13560 = DIRECTION ( 'NONE',  ( -1.000000000000000000, 0.000000000000000000, -0.000000000000000000 ) ) ;
#13561 = EDGE_CURVE ( 'NONE', #19529, #16240, #21291, .T. ) ;
#13562 = FACE_OUTER_BOUND ( 'NONE', #7939, .T. ) ;
#13563 = DIRECTION ( 'NONE',  ( -1.000000000000000000, 0.000000000000000000, 0.000000000000000000 ) ) ;
#13564 = CARTESIAN_POINT ( 'NONE',  ( 1.999999999999994449, 45.00000000000000000, 27.00000000000000000 ) ) ;
#13565 = CARTESIAN_POINT ( 'NONE',  ( -5.871322893124554021, 8.081182679343978492, -3.906742014460231616 ) ) ;
#13566 = ORIENTED_EDGE ( 'NONE', *, *, #13667, .F. ) ;
#13567 = CARTESIAN_POINT ( 'NONE',  ( 41.50000000000000000, -28.80990663662250739, 11.00000000000000000 ) ) ;
#13568 = EDGE_CURVE ( 'NONE', #19937, #5912, #638, .T. ) ;
#13569 = CARTESIAN_POINT ( 'NONE',  ( 5.365059087798939252, 7.384370330707087149, 6.933165578109188765 ) ) ;
#13570 = EDGE_CURVE ( 'NONE', #23352, #22892, #1798, .T. ) ;
#13571 = CARTESIAN_POINT ( 'NONE',  ( 71.67068093254673045, 6.123233995736675563E-16, -5.000000000000007994 ) ) ;
#13572 = CARTESIAN_POINT ( 'NONE',  ( 57.42022815836235594, 7.420530141404717394E-15, 0.000000000000000000 ) ) ;
#13573 = AXIS2_PLACEMENT_3D ( 'NONE', #3859, #15066, #213 ) ;
#13574 = ORIENTED_EDGE ( 'NONE', *, *, #902, .F. ) ;
#13575 = AXIS2_PLACEMENT_3D ( 'NONE', #6229, #15372, #6117 ) ;
#13576 = ORIENTED_EDGE ( 'NONE', *, *, #16470, .T. ) ;
#13577 = ITEM_DEFINED_TRANSFORMATION ( 'NONE', 'NONE', #18172,  #8005 ) ;
#13578 = CARTESIAN_POINT ( 'NONE',  ( 0.000000000000000000, 0.000000000000000000, 0.000000000000000000 ) ) ;
#13579 = CARTESIAN_POINT ( 'NONE',  ( 7.685661446561619314, 5.583959896779020049, -11.40674201446023517 ) ) ;
#13580 = VERTEX_POINT ( 'NONE', #8335 ) ;
#13581 = ORIENTED_EDGE ( 'NONE', *, *, #23958, .F. ) ;
#13582 = ORIENTED_EDGE ( 'NONE', *, *, #4150, .F. ) ;
#13583 = ADVANCED_FACE ( 'NONE', ( #21527 ), #12100, .F. ) ;
#13584 = ORIENTED_EDGE ( 'NONE', *, *, #1498, .T. ) ;
#13585 = CARTESIAN_POINT ( 'NONE',  ( -24.75000000000000000, 29.50000000000000000, 14.00000000000000178 ) ) ;
#13586 = DIRECTION ( 'NONE',  ( -1.000000000000000000, -0.000000000000000000, -0.000000000000000000 ) ) ;
#13587 = DIRECTION ( 'NONE',  ( -0.000000000000000000, -0.000000000000000000, -1.000000000000000000 ) ) ;
#13588 = AXIS2_PLACEMENT_3D ( 'NONE', #8425, #866, #17948 ) ;
#13589 = PRODUCT_DEFINITION_CONTEXT ( 'detailed design', #14630, 'design' ) ;
#13590 = DIRECTION ( 'NONE',  ( -1.000000000000000000, 0.000000000000000000, 0.000000000000000000 ) ) ;
#13591 = ORIENTED_EDGE ( 'NONE', *, *, #21903, .T. ) ;
#13592 = CARTESIAN_POINT ( 'NONE',  ( -36.00000000000001421, 50.99999999999999289, 12.50000000000000000 ) ) ;
#13593 = CARTESIAN_POINT ( 'NONE',  ( 58.87477361290780919, -9.244463733058732095E-30, 5.000000000000007994 ) ) ;
#13594 = VERTEX_POINT ( 'NONE', #4830 ) ;
#13595 = VERTEX_POINT ( 'NONE', #10522 ) ;
#13596 = CARTESIAN_POINT ( 'NONE',  ( -7.685661446562381371, 5.583959896777970222, 10.85958914175814449 ) ) ;
#13597 = ORIENTED_EDGE ( 'NONE', *, *, #23603, .T. ) ;
#13598 = VERTEX_POINT ( 'NONE', #8199 ) ;
#13599 = ORIENTED_EDGE ( 'NONE', *, *, #14113, .F. ) ;
#13600 = CARTESIAN_POINT ( 'NONE',  ( 9.500000000000000000, 6.470877716354879437E-13, -12.63316557810918894 ) ) ;
#13601 = CARTESIAN_POINT ( 'NONE',  ( -2.682529543900285862, 8.255977015246234174, -7.233165578109188587 ) ) ;
#13602 =( BOUNDED_CURVE ( )  B_SPLINE_CURVE ( 2, ( #509, #7685, #6234, #2702, #13675, #15608, #283, #7927, #13297, #15123, #10000 ),
 .UNSPECIFIED., .F., .T. ) 
 B_SPLINE_CURVE_WITH_KNOTS ( ( 3, 2, 2, 2, 2, 3 ),
 ( 0.4999999999999999445, 0.5200000000000000178, 0.5400000000000000355, 0.5600000000000000533, 0.5800000000000000711, 0.6000000000000000888 ),
 .UNSPECIFIED. ) 
 CURVE ( )  GEOMETRIC_REPRESENTATION_ITEM ( )  RATIONAL_B_SPLINE_CURVE ( ( 1.000000000000000000, 0.9510565162951533091, 1.000000000000000000, 0.9510565162951535312, 1.000000000000000000, 0.9510565162951535312, 1.000000000000000000, 0.9510565162951535312, 1.000000000000000000, 0.9510565162951533091, 1.000000000000000222 ) ) 
 REPRESENTATION_ITEM ( '' )  );
#13603 = PRODUCT_DEFINITION ( 'UNKNOWN', '', #20904, #19127 ) ;
#13604 = CARTESIAN_POINT ( 'NONE',  ( 23.00000000000000000, 12.00453763395396756, -1.558955687733494244 ) ) ;
#13605 = ORIENTED_EDGE ( 'NONE', *, *, #22149, .T. ) ;
#13606 = DIRECTION ( 'NONE',  ( 1.000000000000000000, 0.000000000000000000, 0.000000000000000000 ) ) ;
#13607 = CARTESIAN_POINT ( 'NONE',  ( 23.00000000000000000, -9.239931321968246181, 10.79948145182496511 ) ) ;
#13608 = CYLINDRICAL_SURFACE ( 'NONE', #17191, 5.000000000000000888 ) ;
#13609 = CYLINDRICAL_SURFACE ( 'NONE', #4673, 1.000000000000000222 ) ;
#13610 = ORIENTED_EDGE ( 'NONE', *, *, #21785, .T. ) ;
#13611 = FACE_OUTER_BOUND ( 'NONE', #14812, .T. ) ;
#13612 = ADVANCED_FACE ( 'NONE', ( #23253 ), #17378, .F. ) ;
#13613 = LINE ( 'NONE', #18741, #21579 ) ;
#13614 = ADVANCED_FACE ( 'NONE', ( #12240 ), #19711, .T. ) ;
#13615 = ADVANCED_FACE ( 'NONE', ( #24065 ), #7342, .T. ) ;
#13616 = VERTEX_POINT ( 'NONE', #3693 ) ;
#13617 = CARTESIAN_POINT ( 'NONE',  ( 23.00000000000000000, 12.00453763395396756, -7.608955687739546114 ) ) ;
#13618 = CARTESIAN_POINT ( 'NONE',  ( -14.99999999999999645, 15.50000000000000178, 19.70000000000000284 ) ) ;
#13619 = CIRCLE ( 'NONE', #17124, 18.49999999999999645 ) ;
#13620 = FACE_OUTER_BOUND ( 'NONE', #14471, .T. ) ;
#13621 = CARTESIAN_POINT ( 'NONE',  ( 5.365059087799947335, -7.384370330706356178, -6.333165578109188232 ) ) ;
#13622 = CARTESIAN_POINT ( 'NONE',  ( 2.935661446562616295, -9.035036904803758873, 8.806742014460233747 ) ) ;
#13623 = VERTEX_POINT ( 'NONE', #9286 ) ;
#13624 = EDGE_LOOP ( 'NONE', ( #10461, #7813, #16634, #23702, #14720 ) ) ;
#13625 = CARTESIAN_POINT ( 'NONE',  ( -6.153822176767817416E-13, 9.500000000000000000, 3.706742014460232326 ) ) ;
#13626 = ORIENTED_EDGE ( 'NONE', *, *, #23363, .T. ) ;
#13627 = CARTESIAN_POINT ( 'NONE',  ( 8.000000000000021316, 0.000000000000000000, 0.000000000000000000 ) ) ;
#13628 = ORIENTED_EDGE ( 'NONE', *, *, #13207, .T. ) ;
#13629 = CARTESIAN_POINT ( 'NONE',  ( 7.685661446562381371, -5.583959896777971110, -9.859589141758144493 ) ) ;
#13630 = EDGE_CURVE ( 'NONE', #12835, #15166, #14547, .T. ) ;
#13631 = CIRCLE ( 'NONE', #5075, 8.000000000000000000 ) ;
#13632 = DIRECTION ( 'NONE',  ( -1.000000000000000000, -1.224606353822377258E-16, -0.000000000000000000 ) ) ;
#13633 = CARTESIAN_POINT ( 'NONE',  ( 8.871028110654306076, 6.042456644462176420E-13, 12.50000000000000000 ) ) ;
#13634 = DIRECTION ( 'NONE',  ( 0.000000000000000000, -0.4999999999999992784, 0.8660254037844390407 ) ) ;
#13635 = ORIENTED_EDGE ( 'NONE', *, *, #4262, .T. ) ;
#13636 = ORIENTED_EDGE ( 'NONE', *, *, #20878, .T. ) ;
#13637 = DIRECTION ( 'NONE',  ( 0.000000000000000000, -1.000000000000000000, 0.000000000000000000 ) ) ;
#13638 = ADVANCED_FACE ( 'NONE', ( #23957 ), #10872, .F. ) ;
#13639 = DIRECTION ( 'NONE',  ( -0.000000000000000000, -0.000000000000000000, -1.000000000000000000 ) ) ;
#13640 = EDGE_CURVE ( 'NONE', #1207, #14734, #14524, .T. ) ;
#13641 = CARTESIAN_POINT ( 'NONE',  ( -29.00000000000000000, -29.49999999999999645, 12.00000000000000000 ) ) ;
#13642 = EDGE_CURVE ( 'NONE', #14126, #16085, #1406, .T. ) ;
#13643 = DIRECTION ( 'NONE',  ( 0.000000000000000000, 0.000000000000000000, 1.000000000000000000 ) ) ;
#13644 = DIRECTION ( 'NONE',  ( -0.5735764363510517105, -0.8191520442889879128, 0.000000000000000000 ) ) ;
#13645 = EDGE_CURVE ( 'NONE', #17969, #15740, #6870, .T. ) ;
#13646 = DIRECTION ( 'NONE',  ( 0.000000000000000000, 0.000000000000000000, 1.000000000000000000 ) ) ;
#13647 = CARTESIAN_POINT ( 'NONE',  ( 9.500000000000209610, -3.086737114211962396, 5.106742014460234458 ) ) ;
#13648 = VERTEX_POINT ( 'NONE', #22371 ) ;
#13649 = CARTESIAN_POINT ( 'NONE',  ( 7.022953521755574080, -5.102474405759714671, -6.433165578109188765 ) ) ;
#13650 = ORIENTED_EDGE ( 'NONE', *, *, #5697, .T. ) ;
#13651 = VERTEX_POINT ( 'NONE', #12593 ) ;
#13652 = AXIS2_PLACEMENT_3D ( 'NONE', #15614, #23081, #8763 ) ;
#13653 = CARTESIAN_POINT ( 'NONE',  ( -7.685661446562381371, 5.583959896777970222, 10.85958914175814449 ) ) ;
#13654 = CARTESIAN_POINT ( 'NONE',  ( 6.809999908187194197E-13, -9.988891130263535700, 12.70674201446023410 ) ) ;
#13655 = ORIENTED_EDGE ( 'NONE', *, *, #8439, .T. ) ;
#13656 = DIRECTION ( 'NONE',  ( -1.000000000000000000, -1.224606353822377258E-16, -0.000000000000000000 ) ) ;
#13657 = LINE ( 'NONE', #8528, #16627 ) ;
#13658 = CARTESIAN_POINT ( 'NONE',  ( -5.871322893124554021, 8.081182679343978492, 6.759589141758143072 ) ) ;
#13659 = EDGE_CURVE ( 'NONE', #3340, #18614, #16591, .T. ) ;
#13660 = CARTESIAN_POINT ( 'NONE',  ( 63.23840997654417606, 7.420530141404717394E-15, 0.000000000000000000 ) ) ;
#13661 = DIRECTION ( 'NONE',  ( -1.000000000000000000, 0.000000000000000000, 0.000000000000000000 ) ) ;
#13662 = FACE_OUTER_BOUND ( 'NONE', #11632, .T. ) ;
#13663 = CARTESIAN_POINT ( 'NONE',  ( 78.94340820527399671, -5.000000000000000888, 6.123233995736776143E-16 ) ) ;
#13664 = VERTEX_POINT ( 'NONE', #5293 ) ;
#13665=STYLED_ITEM('',(#24155),#18330);
#13666 = DIRECTION ( 'NONE',  ( 0.000000000000000000, 0.000000000000000000, -1.000000000000000000 ) ) ;
#13667 = EDGE_CURVE ( 'NONE', #14408, #8124, #20113, .T. ) ;
#13668 = EDGE_CURVE ( 'NONE', #17477, #2565, #8824, .T. ) ;
#13669 = ORIENTED_EDGE ( 'NONE', *, *, #7469, .F. ) ;
#13670 = FACE_OUTER_BOUND ( 'NONE', #3958, .T. ) ;
#13671 = CARTESIAN_POINT ( 'NONE',  ( -5.871322893123449127, -8.081182679344781405, 11.35958914175814272 ) ) ;
#13672 = PRESENTATION_STYLE_ASSIGNMENT (( #11584 ) ) ;
#13673 = LINE ( 'NONE', #20755, #2722 ) ;
#13674 = CARTESIAN_POINT ( 'NONE',  ( -31.74999999999995737, 0.000000000000000000, 0.000000000000000000 ) ) ;
#13675 = CARTESIAN_POINT ( 'NONE',  ( -2.935661446562617183, 9.035036904803758873, -7.806742014460233747 ) ) ;
#13676 = CARTESIAN_POINT ( 'NONE',  ( -6.822232771736904647E-13, 9.988891130263535700, 8.559589141758142006 ) ) ;
#13677 = ORIENTED_EDGE ( 'NONE', *, *, #17495, .T. ) ;
#13678 = CARTESIAN_POINT ( 'NONE',  ( 5.871322893124553133, -8.081182679343980269, -6.906742014460234280 ) ) ;
#13679 = ORIENTED_EDGE ( 'NONE', *, *, #4935, .F. ) ;
#13680 = DIRECTION ( 'NONE',  ( 0.000000000000000000, -1.000000000000000000, 0.000000000000000000 ) ) ;
#13681 = CARTESIAN_POINT ( 'NONE',  ( 7.022953521755574080, -5.102474405759714671, 6.433165578109188765 ) ) ;
#13682 = CARTESIAN_POINT ( 'NONE',  ( 23.00000000000000000, -3.205857990849823480, 11.23818298448541420 ) ) ;
#13683 = CARTESIAN_POINT ( 'NONE',  ( -2.000000000000000000, 0.000000000000000000, 0.4999999999999995559 ) ) ;
#13684 = AXIS2_PLACEMENT_3D ( 'NONE', #3531, #21841, #1831 ) ;
#13685 = ORIENTED_EDGE ( 'NONE', *, *, #13755, .T. ) ;
#13686 = ORIENTED_EDGE ( 'NONE', *, *, #1725, .F. ) ;
#13687 = DIRECTION ( 'NONE',  ( -0.000000000000000000, -0.000000000000000000, -1.000000000000000000 ) ) ;
#13688 = VERTEX_POINT ( 'NONE', #23723 ) ;
#13689 = ORIENTED_EDGE ( 'NONE', *, *, #8242, .T. ) ;
#13690 = CARTESIAN_POINT ( 'NONE',  ( -4.632213926375346347, -7.938484784988568244, -12.31707955932596477 ) ) ;
#13691 = ADVANCED_FACE ( 'NONE', ( #20290, #6991 ), #3339, .F. ) ;
#13692 = CARTESIAN_POINT ( 'NONE',  ( 0.000000000000000000, 11.58003564732003277, -1.573866785045813010 ) ) ;
#13693 = ORIENTED_EDGE ( 'NONE', *, *, #3612, .F. ) ;
#13694 = CIRCLE ( 'NONE', #19564, 5.000000000000007994 ) ;
#13695 = AXIS2_PLACEMENT_3D ( 'NONE', #4777, #8285, #15739 ) ;
#13696 = VERTEX_POINT ( 'NONE', #1518 ) ;
#13697 = CARTESIAN_POINT ( 'NONE',  ( -7.685661446561619314, -5.583959896779019161, 10.40674201446023339 ) ) ;
#13698 = LINE ( 'NONE', #4451, #4797 ) ;
#13699 = VECTOR ( 'NONE', #20083, 1000.000000000000000 ) ;
#13700 = FACE_OUTER_BOUND ( 'NONE', #3775, .T. ) ;
#13701 = DIRECTION ( 'NONE',  ( -0.000000000000000000, -0.000000000000000000, -1.000000000000000000 ) ) ;
#13702 = ORIENTED_EDGE ( 'NONE', *, *, #14661, .T. ) ;
#13703 = DIRECTION ( 'NONE',  ( 0.000000000000000000, -1.000000000000000000, 0.000000000000000000 ) ) ;
#13704 = DIRECTION ( 'NONE',  ( 1.000000000000000000, 0.000000000000000000, 0.000000000000000000 ) ) ;
#13705 = ORIENTED_EDGE ( 'NONE', *, *, #186, .T. ) ;
#13706 = ORIENTED_EDGE ( 'NONE', *, *, #20845, .T. ) ;
#13707 = CARTESIAN_POINT ( 'NONE',  ( 2.935661446561383503, 9.035036904804158553, 6.459589141758144137 ) ) ;
#13708 = EDGE_LOOP ( 'NONE', ( #8732, #18578 ) ) ;
#13709 = ORIENTED_EDGE ( 'NONE', *, *, #16785, .F. ) ;
#13710 = VERTEX_POINT ( 'NONE', #3461 ) ;
#13711 = ADVANCED_FACE ( 'NONE', ( #12721 ), #8931, .F. ) ;
#13712 = AXIS2_PLACEMENT_3D ( 'NONE', #13129, #13369, #20831 ) ;
#13713 = EDGE_LOOP ( 'NONE', ( #21645, #12933, #18566, #5902, #6590 ) ) ;
#13714 = AXIS2_PLACEMENT_3D ( 'NONE', #2325, #22953, #11818 ) ;
#13715 = EDGE_CURVE ( 'NONE', #20352, #9356, #19322, .T. ) ;
#13716 = VERTEX_POINT ( 'NONE', #9175 ) ;
#13717 = CARTESIAN_POINT ( 'NONE',  ( 29.00000000000000000, -29.50000000000000355, 12.00000000000000000 ) ) ;
#13719 = AXIS2_PLACEMENT_3D ( 'NONE', #11561, #19030, #11793 ) ;
#13718 = CARTESIAN_POINT ( 'NONE',  ( -2.682529543900285862, 8.255977015246234174, -5.233165578109188587 ) ) ;
#13720 = AXIS2_PLACEMENT_3D ( 'NONE', #19448, #14070, #11862 ) ;
#13721 = CIRCLE ( 'NONE', #19181, 6.050000000006050982 ) ;
#13722 = EDGE_CURVE ( 'NONE', #3260, #14186, #16626, .T. ) ;
#13723 = VERTEX_POINT ( 'NONE', #20405 ) ;
#13724 = CARTESIAN_POINT ( 'NONE',  ( 0.000000000000000000, 12.00453763395396756, -7.608955687739546114 ) ) ;
#13725 = CARTESIAN_POINT ( 'NONE',  ( 0.000000000000000000, 45.00000000000000000, 26.97499999999999432 ) ) ;
#13726 = AXIS2_PLACEMENT_3D ( 'NONE', #7233, #15015, #23955 ) ;
#13727 = CARTESIAN_POINT ( 'NONE',  ( 62.94340820527399671, 7.562528597612068045E-15, 0.000000000000000000 ) ) ;
#13728 = EDGE_CURVE ( 'NONE', #831, #13080, #1967, .T. ) ;
#13729 = PLANE ( 'NONE',  #23965 ) ;
#13730 = FACE_OUTER_BOUND ( 'NONE', #13383, .T. ) ;
#13731 = ORIENTED_EDGE ( 'NONE', *, *, #4338, .F. ) ;
#13732 = LINE ( 'NONE', #11892, #2173 ) ;
#13733 = DIRECTION ( 'NONE',  ( -0.000000000000000000, 1.295896757998780388E-15, 1.000000000000000000 ) ) ;
#13734 = VERTEX_POINT ( 'NONE', #2339 ) ;
#13735 = CARTESIAN_POINT ( 'NONE',  ( 21.13207267780287069, 38.32709852940855910, 0.000000000000000000 ) ) ;
#13736 = DIRECTION ( 'NONE',  ( -1.000000000000000000, 0.000000000000000000, 0.000000000000000000 ) ) ;
#13737 = AXIS2_PLACEMENT_3D ( 'NONE', #20114, #14595, #3748 ) ;
#13738 = DIRECTION ( 'NONE',  ( 0.000000000000000000, 0.000000000000000000, 1.000000000000000000 ) ) ;
#13739 = CARTESIAN_POINT ( 'NONE',  ( -6.233975306307045953E-13, 9.127583699786111282, -5.133165578109188054 ) ) ;
#13740 = CIRCLE ( 'NONE', #2029, 5.000000000000007994 ) ;
#13741 = VECTOR ( 'NONE', #5027, 1000.000000000000000 ) ;
#13742 = AXIS2_PLACEMENT_3D ( 'NONE', #15867, #14034, #17556 ) ;
#13743 = CIRCLE ( 'NONE', #18433, 6.050000000006050982 ) ;
#13744 = DIRECTION ( 'NONE',  ( -6.938893903907222856E-15, -1.000000000000000000, 0.000000000000000000 ) ) ;
#13745 = ORIENTED_EDGE ( 'NONE', *, *, #12494, .F. ) ;
#13746 = ORIENTED_EDGE ( 'NONE', *, *, #15903, .F. ) ;
#13747 = AXIS2_PLACEMENT_3D ( 'NONE', #5491, #9262, #16709 ) ;
#13748 = VERTEX_POINT ( 'NONE', #15016 ) ;
#13749 =( BOUNDED_SURFACE ( )  B_SPLINE_SURFACE ( 1, 2, ( 
 ( #8181, #22978, #22867, #15624, #406, #10132, #20910, #23093, #4681, #2349, #19324, #12084, #19557, #17585, #4439, #11603, #889, #9898, #13579, #6382, #19073, #10016, #15513, #22732, #6513, #13825, #2719, #7812, #6016, #660, #21274, #9762, #21021, #8316, #6138, #13455, #528, #15253, #11969, #17222, #4196, #15396, #4310, #2832, #11715, #8067, #15770, #2474, #17357, #23235, #13950, #6249, #17104, #17967, #21756, #5046, #8916, #14528, #14061, #12344, #18096, #4931, #21508, #16357, #17855, #19814, #14176, #2971, #1389, #3086, #10506, #8556, #21993, #1254, #23815, #20169, #10268, #12458, #8675, #23709, #5275, #16002, #21635, #3192, #12572, #10400, #23594, #16131, #6872, #19919, #8808, #14295, #16252, #6980, #21866, #12706, #5146 ),
 ( #20044, #3325, #10747, #18216, #1141, #1506, #6744, #7089, #17724, #1027, #8448, #15896, #23355, #2076, #12931, #16957, #1732, #10856, #3909, #23941, #5500, #9033, #13286, #5859, #13170, #18324, #14875, #11090, #20386, #12817, #5755, #18794, #20525, #16482, #7214, #3678, #18574, #7431, #14657, #22351, #9373, #5395, #14998, #22127, #24, #3549, #20627, #10963, #7675, #7552, #22479, #11317, #5632, #13059, #9503, #1850, #272, #3798, #9270, #15113, #18443, #18679, #11207, #22578, #3445, #16717, #1609, #1951, #20274, #16825, #144, #9158, #16607, #24051, #7330, #14770, #22230, #17557, #15486, #21106, #23063, #13424, #20882, #18927, #745, #22696, #497, #15363, #2441, #4172, #9867, #4410, #859, #11451, #9988, #9629, #17324 ) ),
 .UNSPECIFIED., .F., .F., .T. ) 
 B_SPLINE_SURFACE_WITH_KNOTS ( ( 2, 2 ),
 ( 3, 2, 2, 2, 2, 2, 2, 2, 2, 2, 2, 2, 2, 2, 2, 2, 2, 2, 2, 2, 2, 2, 2, 2, 2, 2, 2, 2, 2, 2, 2, 2, 2, 2, 2, 2, 2, 2, 2, 2, 2, 2, 2, 2, 2, 2, 2, 2, 3 ),
 ( 0.000000000000000000, 1.000000000000000000 ),
 ( 0.000000000000000000, 0.02000000000000000042, 0.04000000000000000083, 0.05999999999999999778, 0.08000000000000000167, 0.1000000000000000056, 0.1199999999999999956, 0.1400000000000000133, 0.1600000000000000033, 0.1799999999999999933, 0.2000000000000000111, 0.2200000000000000011, 0.2399999999999999911, 0.2600000000000000089, 0.2800000000000000266, 0.2999999999999999889, 0.3200000000000000067, 0.3400000000000000244, 0.3599999999999999867, 0.3800000000000000044, 0.4000000000000000222, 0.4199999999999999845, 0.4400000000000000022, 0.4600000000000000200, 0.4799999999999999822, 0.5000000000000000000, 0.5200000000000000178, 0.5400000000000000355, 0.5600000000000000533, 0.5799999999999999600, 0.5999999999999999778, 0.6199999999999999956, 0.6400000000000000133, 0.6600000000000000311, 0.6800000000000000488, 0.6999999999999999556, 0.7199999999999999734, 0.7399999999999999911, 0.7600000000000000089, 0.7800000000000000266, 0.8000000000000000444, 0.8199999999999999512, 0.8399999999999999689, 0.8599999999999999867, 0.8800000000000000044, 0.9000000000000000222, 0.9200000000000000400, 0.9399999999999999467, 0.9500000000000000666 ),
 .UNSPECIFIED. ) 
 GEOMETRIC_REPRESENTATION_ITEM ( )  RATIONAL_B_SPLINE_SURFACE ( (
 ( 1.000000000000000000, 0.9510565162951535312, 1.000000000000000000, 0.9510565162951535312, 1.000000000000000000, 0.9510565162951535312, 1.000000000000000000, 0.9510565162951535312, 1.000000000000000000, 0.9510565162951535312, 1.000000000000000000, 0.9510565162951535312, 1.000000000000000000, 0.9510565162951535312, 1.000000000000000000, 0.9510565162951535312, 1.000000000000000000, 0.9510565162951535312, 1.000000000000000000, 0.9510565162951535312, 1.000000000000000000, 0.9510565162951535312, 1.000000000000000000, 0.9510565162951535312, 1.000000000000000000, 0.9510565162951535312, 1.000000000000000000, 0.9510565162951535312, 1.000000000000000000, 0.9510565162951535312, 1.000000000000000000, 0.9510565162951535312, 1.000000000000000000, 0.9510565162951535312, 1.000000000000000000, 0.9510565162951535312, 1.000000000000000000, 0.9510565162951535312, 1.000000000000000000, 0.9510565162951535312, 1.000000000000000000, 0.9510565162951535312, 1.000000000000000000, 0.9510565162951535312, 1.000000000000000000, 0.9510565162951535312, 1.000000000000000000, 0.9510565162951535312, 1.000000000000000000, 0.9510565162951535312, 1.000000000000000000, 0.9510565162951535312, 1.000000000000000000, 0.9510565162951535312, 1.000000000000000000, 0.9510565162951535312, 1.000000000000000000, 0.9510565162951535312, 1.000000000000000000, 0.9510565162951535312, 1.000000000000000000, 0.9510565162951535312, 1.000000000000000000, 0.9510565162951535312, 1.000000000000000000, 0.9510565162951535312, 1.000000000000000000, 0.9510565162951535312, 1.000000000000000000, 0.9510565162951535312, 1.000000000000000000, 0.9510565162951535312, 1.000000000000000000, 0.9510565162951535312, 1.000000000000000000, 0.9510565162951535312, 1.000000000000000000, 0.9510565162951535312, 1.000000000000000000, 0.9510565162951535312, 1.000000000000000000, 0.9510565162951535312, 1.000000000000000000, 0.9510565162951535312, 1.000000000000000000, 0.9510565162951535312, 1.000000000000000000, 0.9510565162951535312, 1.000000000000000000, 0.9510565162951535312, 1.000000000000000000, 0.9510565162951535312, 1.000000000000000000, 0.9510565162951535312, 1.000000000000000000, 0.9755282581475764880, 0.9755282581475768211),
 ( 1.000000000000000000, 0.9510565162951535312, 1.000000000000000000, 0.9510565162951535312, 1.000000000000000000, 0.9510565162951535312, 1.000000000000000000, 0.9510565162951535312, 1.000000000000000000, 0.9510565162951535312, 1.000000000000000000, 0.9510565162951535312, 1.000000000000000000, 0.9510565162951535312, 1.000000000000000000, 0.9510565162951535312, 1.000000000000000000, 0.9510565162951535312, 1.000000000000000000, 0.9510565162951535312, 1.000000000000000000, 0.9510565162951535312, 1.000000000000000000, 0.9510565162951535312, 1.000000000000000000, 0.9510565162951535312, 1.000000000000000000, 0.9510565162951535312, 1.000000000000000000, 0.9510565162951535312, 1.000000000000000000, 0.9510565162951535312, 1.000000000000000000, 0.9510565162951535312, 1.000000000000000000, 0.9510565162951535312, 1.000000000000000000, 0.9510565162951535312, 1.000000000000000000, 0.9510565162951535312, 1.000000000000000000, 0.9510565162951535312, 1.000000000000000000, 0.9510565162951535312, 1.000000000000000000, 0.9510565162951535312, 1.000000000000000000, 0.9510565162951535312, 1.000000000000000000, 0.9510565162951535312, 1.000000000000000000, 0.9510565162951535312, 1.000000000000000000, 0.9510565162951535312, 1.000000000000000000, 0.9510565162951535312, 1.000000000000000000, 0.9510565162951535312, 1.000000000000000000, 0.9510565162951535312, 1.000000000000000000, 0.9510565162951535312, 1.000000000000000000, 0.9510565162951535312, 1.000000000000000000, 0.9510565162951535312, 1.000000000000000000, 0.9510565162951535312, 1.000000000000000000, 0.9510565162951535312, 1.000000000000000000, 0.9510565162951535312, 1.000000000000000000, 0.9510565162951535312, 1.000000000000000000, 0.9510565162951535312, 1.000000000000000000, 0.9510565162951535312, 1.000000000000000000, 0.9510565162951535312, 1.000000000000000000, 0.9510565162951535312, 1.000000000000000000, 0.9510565162951535312, 1.000000000000000000, 0.9510565162951535312, 1.000000000000000000, 0.9510565162951535312, 1.000000000000000000, 0.9510565162951535312, 1.000000000000000000, 0.9510565162951535312, 1.000000000000000000, 0.9510565162951535312, 1.000000000000000000, 0.9755282581475764880, 0.9755282581475768211) ) ) 
 REPRESENTATION_ITEM ( '' )  SURFACE ( )  );
#13750 = CARTESIAN_POINT ( 'NONE',  ( 5.871322893123448239, 8.081182679344781405, -11.50674201446023126 ) ) ;
#13751 = EDGE_LOOP ( 'NONE', ( #4502, #3899, #3252, #9180 ) ) ;
#13752 = ADVANCED_FACE ( 'NONE', ( #13303 ), #16976, .F. ) ;
#13753 = CARTESIAN_POINT ( 'NONE',  ( 9.500000000000209610, -3.086737114211962396, -9.959589141758145914 ) ) ;
#13754 = UNCERTAINTY_MEASURE_WITH_UNIT (LENGTH_MEASURE( 1.000000000000000082E-05 ), #11770, 'distance_accuracy_value', 'NONE');
#13755 = EDGE_CURVE ( 'NONE', #7176, #6097, #19365, .T. ) ;
#13756 = CARTESIAN_POINT ( 'NONE',  ( 7.524481829284360046, -4.467250836390474156, 12.50000000000000178 ) ) ;
#13758 = AXIS2_PLACEMENT_3D ( 'NONE', #11211, #18134, #23844 ) ;
#13757 = CARTESIAN_POINT ( 'NONE',  ( -9.500000000000211386, 3.086737114211961064, 4.106742014460232681 ) ) ;
#13759 = CIRCLE ( 'NONE', #16093, 6.050000000006052758 ) ;
#13760 = ORIENTED_EDGE ( 'NONE', *, *, #6830, .T. ) ;
#13761 = DIRECTION ( 'NONE',  ( -0.000000000000000000, -0.000000000000000000, -1.000000000000000000 ) ) ;
#13762 = AXIS2_PLACEMENT_3D ( 'NONE', #23750, #12624, #7134 ) ;
#13763 = DIRECTION ( 'NONE',  ( -1.000000000000000000, -1.224606353822377258E-16, -0.000000000000000000 ) ) ;
#13764 = AXIS2_PLACEMENT_3D ( 'NONE', #7441, #15126, #161 ) ;
#13765 = CYLINDRICAL_SURFACE ( 'NONE', #5642, 5.000000000000000888 ) ;
#13766 = ORIENTED_EDGE ( 'NONE', *, *, #11291, .F. ) ;
#13767 = DIRECTION ( 'NONE',  ( 0.000000000000000000, 0.000000000000000000, -1.000000000000000000 ) ) ;
#13768 = LINE ( 'NONE', #6321, #16070 ) ;
#13769 = AXIS2_PLACEMENT_3D ( 'NONE', #9958, #10077, #8243 ) ;
#13770 = DIRECTION ( 'NONE',  ( -1.000000000000000000, -1.224606353822377258E-16, -0.000000000000000000 ) ) ;
#13771 = CARTESIAN_POINT ( 'NONE',  ( -34.00000000000000000, 3.999999999999999112, 10.49999999999999822 ) ) ;
#13772 = EDGE_LOOP ( 'NONE', ( #9458, #7567, #9684 ) ) ;
#13773 = CARTESIAN_POINT ( 'NONE',  ( -7.022953521754877748, -5.102474405760673015, -5.833165578109188232 ) ) ;
#13774 = PRODUCT_DEFINITION ( 'UNKNOWN', '', #2202, #4319 ) ;
#13775 = EDGE_LOOP ( 'NONE', ( #21742, #1514, #11653, #6485 ) ) ;
#13776 = AXIS2_PLACEMENT_3D ( 'NONE', #20888, #15369, #4177 ) ;
#13777 = CARTESIAN_POINT ( 'NONE',  ( 5.078177448618334644, 0.000000000000000000, 0.000000000000000000 ) ) ;
#13778 = CARTESIAN_POINT ( 'NONE',  ( 0.000000000000000000, 0.000000000000000000, 0.000000000000000000 ) ) ;
#13779 = AXIS2_PLACEMENT_3D ( 'NONE', #10142, #4581, #17599 ) ;
#13780 = VERTEX_POINT ( 'NONE', #9646 ) ;
#13781 =( NAMED_UNIT ( * ) SI_UNIT ( $, .STERADIAN. ) SOLID_ANGLE_UNIT ( ) );
#13782 = EDGE_CURVE ( 'NONE', #23345, #17607, #2225, .T. ) ;
#13783 = CARTESIAN_POINT ( 'NONE',  ( 2.682529543900284974, -8.255977015246234174, -12.23316557810919036 ) ) ;
#13784 = AXIS2_PLACEMENT_3D ( 'NONE', #12605, #20072, #16716 ) ;
#13785 = CARTESIAN_POINT ( 'NONE',  ( 74.00000000000001421, 4.172000000000015696, 0.000000000000000000 ) ) ;
#13786 = ADVANCED_FACE ( 'NONE', ( #8907 ), #7625, .F. ) ;
#13787 = CIRCLE ( 'NONE', #4445, 8.000000000000000000 ) ;
#13788 = DIRECTION ( 'NONE',  ( 0.000000000000000000, -1.000000000000000000, 0.000000000000000000 ) ) ;
#13789 = ADVANCED_FACE ( 'NONE', ( #5264 ), #13499, .T. ) ;
#13790 = PLANE ( 'NONE',  #532 ) ;
#13791 = DIRECTION ( 'NONE',  ( 0.000000000000000000, 0.000000000000000000, 1.000000000000000000 ) ) ;
#13792 = DIRECTION ( 'NONE',  ( -0.000000000000000000, -0.000000000000000000, 1.000000000000000000 ) ) ;
#13793 = VERTEX_POINT ( 'NONE', #21981 ) ;
#13794 = ORIENTED_EDGE ( 'NONE', *, *, #5926, .F. ) ;
#13795 = DIRECTION ( 'NONE',  ( 0.000000000000000000, 0.000000000000000000, 1.000000000000000000 ) ) ;
#13796 = CARTESIAN_POINT ( 'NONE',  ( -2.094119113047911540, -8.892932511210149826, 12.37200713923885687 ) ) ;
#13797 = DIRECTION ( 'NONE',  ( 1.000000000000000000, 0.000000000000000000, 0.000000000000000000 ) ) ;
#13798 = AXIS2_PLACEMENT_3D ( 'NONE', #2431, #8271, #2682 ) ;
#13799 = CARTESIAN_POINT ( 'NONE',  ( -29.00000000000000355, -3.851859888774471706E-31, 9.500000000000000000 ) ) ;
#13800 = AXIS2_PLACEMENT_3D ( 'NONE', #21151, #7963, #8333 ) ;
#13801 = ORIENTED_EDGE ( 'NONE', *, *, #21323, .T. ) ;
#13802 = CIRCLE ( 'NONE', #22000, 4.172000000000008590 ) ;
#13803 = AXIS2_PLACEMENT_3D ( 'NONE', #2872, #4964, #10424 ) ;
#13804 = CARTESIAN_POINT ( 'NONE',  ( 4.029965094393306726E-41, -5.916456789157588541E-28, -21.49999999999996803 ) ) ;
#13805 = DIRECTION ( 'NONE',  ( 0.5735764363510424957, 0.8191520442889943521, 0.000000000000000000 ) ) ;
#13806 = VERTEX_POINT ( 'NONE', #12559 ) ;
#13807 = EDGE_CURVE ( 'NONE', #13385, #18344, #10746, .T. ) ;
#13808 = CARTESIAN_POINT ( 'NONE',  ( -9.500000000000000000, -6.482511860946779655E-13, -6.206742014460234103 ) ) ;
#13809 = AXIS2_PLACEMENT_3D ( 'NONE', #6326, #14018, #2557 ) ;
#13810 = EDGE_LOOP ( 'NONE', ( #8632, #5804, #21440, #24003 ) ) ;
#13811 = DIRECTION ( 'NONE',  ( -1.000000000000000000, -0.000000000000000000, -0.000000000000000000 ) ) ;
#13812 = CARTESIAN_POINT ( 'NONE',  ( 7.022953521755574080, -5.102474405759714671, 8.433165578109187877 ) ) ;
#13813 = DIRECTION ( 'NONE',  ( 0.000000000000000000, -1.000000000000000000, 0.000000000000000000 ) ) ;
#13814 = LINE ( 'NONE', #17467, #5549 ) ;
#13815 = CARTESIAN_POINT ( 'NONE',  ( 0.000000000000000000, -45.00000000000000000, 0.02500000000000418554 ) ) ;
#13816 = EDGE_CURVE ( 'NONE', #19098, #8836, #20524, .T. ) ;
#13817 = ADVANCED_FACE ( 'NONE', ( #3314 ), #8807, .T. ) ;
#13818 = ORIENTED_EDGE ( 'NONE', *, *, #22390, .T. ) ;
#13819 = CIRCLE ( 'NONE', #21616, 5.099999999999996980 ) ;
#13820 = TOROIDAL_SURFACE ( 'NONE', #14587, 10.02592346138681023, 0.2999999999999999334 ) ;
#13821 = ORIENTED_EDGE ( 'NONE', *, *, #6120, .F. ) ;
#13822 = ORIENTED_EDGE ( 'NONE', *, *, #10365, .F. ) ;
#13823 = CARTESIAN_POINT ( 'NONE',  ( -41.00000000000000000, 5.000000000000000888, 9.500000000000000000 ) ) ;
#13824 = TOROIDAL_SURFACE ( 'NONE', #2927, 2.000000000000000000, 1.000000000000000000 ) ;
#13825 = CARTESIAN_POINT ( 'NONE',  ( 6.809999908187194197E-13, -9.988891130263535700, -10.70674201446023233 ) ) ;
#13826 = ORIENTED_EDGE ( 'NONE', *, *, #13213, .T. ) ;
#13827 = CIRCLE ( 'NONE', #21622, 8.000000000000000000 ) ;
#13828 = EDGE_LOOP ( 'NONE', ( #19972, #10736, #13925, #23104 ) ) ;
#13829 = CARTESIAN_POINT ( 'NONE',  ( -3.577580068923903234, -8.440353260633020938, -12.34099035630368491 ) ) ;
#13830 = DIRECTION ( 'NONE',  ( 0.000000000000000000, 0.000000000000000000, 1.000000000000000000 ) ) ;
#13831 = VERTEX_POINT ( 'NONE', #5133 ) ;
#13832 = CARTESIAN_POINT ( 'NONE',  ( -2.285357169336379446, -9.225016725403595075, -3.500112653623174364 ) ) ;
#13833 = VERTEX_POINT ( 'NONE', #7075 ) ;
#13834 = CARTESIAN_POINT ( 'NONE',  ( -40.00000000000000000, -29.49999999999999645, 0.000000000000000000 ) ) ;
#13835 = DIRECTION ( 'NONE',  ( 0.000000000000000000, 0.000000000000000000, 1.000000000000000000 ) ) ;
#13836 = DIRECTION ( 'NONE',  ( 1.000000000000000000, 0.000000000000000000, 0.000000000000000000 ) ) ;
#13837 = PRODUCT_DEFINITION_CONTEXT ( 'detailed design', #3874, 'design' ) ;
#13838 = DIRECTION ( 'NONE',  ( 0.000000000000000000, 0.000000000000000000, -1.000000000000000000 ) ) ;
#13839 = ORIENTED_EDGE ( 'NONE', *, *, #681, .F. ) ;
#13840 = CARTESIAN_POINT ( 'NONE',  ( 29.00000000000000355, -29.50000000000000000, -3.000000000000000000 ) ) ;
#13841 = LINE ( 'NONE', #19931, #7155 ) ;
#13842 = DIRECTION ( 'NONE',  ( 0.000000000000000000, 0.000000000000000000, -1.000000000000000000 ) ) ;
#13843 = ORIENTED_EDGE ( 'NONE', *, *, #4827, .T. ) ;
#13844 = AXIS2_PLACEMENT_3D ( 'NONE', #16397, #14440, #5188 ) ;
#13845 = ORIENTED_EDGE ( 'NONE', *, *, #18920, .T. ) ;
#13846 = CARTESIAN_POINT ( 'NONE',  ( 2.935661446561383503, 9.035036904804158553, 8.459589141758144137 ) ) ;
#13847 = EDGE_LOOP ( 'NONE', ( #15343, #20813, #20608, #14462, #16623, #17089, #4358, #11750, #17293, #15561, #4916, #15391, #23471, #8647, #15918, #10950, #1891, #18978, #11480, #2264, #8888, #1128, #11651, #17243 ) ) ;
#13848 = VECTOR ( 'NONE', #20018, 1000.000000000000000 ) ;
#13849 = ORIENTED_EDGE ( 'NONE', *, *, #19333, .F. ) ;
#13850 = ORIENTED_EDGE ( 'NONE', *, *, #15885, .T. ) ;
#13851 = EDGE_CURVE ( 'NONE', #4606, #13385, #14513, .T. ) ;
#13853 = EDGE_CURVE ( 'NONE', #4506, #6894, #13098, .T. ) ;
#13852 = AXIS2_PLACEMENT_3D ( 'NONE', #1714, #17954, #1593 ) ;
#13854 = AXIS2_PLACEMENT_3D ( 'NONE', #17798, #17655, #10456 ) ;
#13855 = EDGE_LOOP ( 'NONE', ( #18751, #903 ) ) ;
#13856 = ORIENTED_EDGE ( 'NONE', *, *, #17516, .F. ) ;
#13857 = VERTEX_POINT ( 'NONE', #9362 ) ;
#13858 = CARTESIAN_POINT ( 'NONE',  ( 58.87477361290780919, 7.420530141404717394E-15, 0.000000000000000000 ) ) ;
#13859 = DIRECTION ( 'NONE',  ( 0.000000000000000000, 0.000000000000000000, 1.000000000000000000 ) ) ;
#13860 = CARTESIAN_POINT ( 'NONE',  ( -14.67187117805616126, -3.178673068337432461, -8.975236025575920706 ) ) ;
#13861 = ORIENTED_EDGE ( 'NONE', *, *, #13816, .F. ) ;
#13862 = CARTESIAN_POINT ( 'NONE',  ( -15.57833309066360350, -5.219313726039664481, 7.987432870209368652 ) ) ;
#13863 = DIRECTION ( 'NONE',  ( -1.000000000000000000, -1.224606353822377258E-16, -0.000000000000000000 ) ) ;
#13865 = DIRECTION ( 'NONE',  ( -1.000000000000000000, -1.224606353822377258E-16, -0.000000000000000000 ) ) ;
#13864 = APPLICATION_CONTEXT ( 'automotive_design' ) ;
#13866 = FACE_OUTER_BOUND ( 'NONE', #18561, .T. ) ;
#13867 = ORIENTED_EDGE ( 'NONE', *, *, #5723, .F. ) ;
#13868 = DIRECTION ( 'NONE',  ( -1.000000000000000000, -1.224606353822377258E-16, -0.000000000000000000 ) ) ;
#13869 = ADVANCED_FACE ( 'NONE', ( #23677 ), #16235, .F. ) ;
#13870 = DIRECTION ( 'NONE',  ( 0.000000000000000000, 0.000000000000000000, 1.000000000000000000 ) ) ;
#13871 = CIRCLE ( 'NONE', #9557, 1.000000000000000888 ) ;
#13872 = CARTESIAN_POINT ( 'NONE',  ( 9.499999999999790390, 3.086737114213260025, 4.159589141758142539 ) ) ;
#13873 = AXIS2_PLACEMENT_3D ( 'NONE', #20181, #14673, #16268 ) ;
#13874 = CARTESIAN_POINT ( 'NONE',  ( 16.68233279685676251, -7.225448002938847480, -6.184784653374910235 ) ) ;
#13875 = CARTESIAN_POINT ( 'NONE',  ( -23.90000000000000568, -29.49999999999999645, 12.00000000000000000 ) ) ;
#13876 = ADVANCED_FACE ( 'NONE', ( #18398 ), #2991, .T. ) ;
#13877 = CARTESIAN_POINT ( 'NONE',  ( 2.682529543899157876, 8.255977015246598327, -7.033165578109189298 ) ) ;
#13878 = CARTESIAN_POINT ( 'NONE',  ( 59.45454545454545325, -4.172000000000000597, 0.000000000000000000 ) ) ;
#13879 = ORIENTED_EDGE ( 'NONE', *, *, #16817, .T. ) ;
#13880 = ORIENTED_EDGE ( 'NONE', *, *, #13417, .F. ) ;
#13881 = ADVANCED_FACE ( 'NONE', ( #22083 ), #19776, .F. ) ;
#13882 = CARTESIAN_POINT ( 'NONE',  ( -2.935661446562617183, 9.035036904803758873, 3.806742014460233303 ) ) ;
#13883 = VECTOR ( 'NONE', #11888, 1000.000000000000000 ) ;
#13884 = ADVANCED_FACE ( 'NONE', ( #14259 ), #9578, .F. ) ;
#13885 = ORIENTED_EDGE ( 'NONE', *, *, #2492, .F. ) ;
#13886 = DIRECTION ( 'NONE',  ( 0.000000000000000000, 0.000000000000000000, 1.000000000000000000 ) ) ;
#13887 =( GEOMETRIC_REPRESENTATION_CONTEXT ( 3 ) GLOBAL_UNCERTAINTY_ASSIGNED_CONTEXT ( ( #13522 ) ) GLOBAL_UNIT_ASSIGNED_CONTEXT ( ( #20478, #12896, #9343 ) ) REPRESENTATION_CONTEXT ( 'NONE', 'WORKASPACE' ) );
#13888 = LINE ( 'NONE', #8006, #10080 ) ;
#13889 = AXIS2_PLACEMENT_3D ( 'NONE', #11656, #4509, #19625 ) ;
#13890 = ORIENTED_EDGE ( 'NONE', *, *, #681, .T. ) ;
#13891 = CARTESIAN_POINT ( 'NONE',  ( 23.00000000000000000, 17.26667456984545979, 4.623588898214379128 ) ) ;
#13892 = LINE ( 'NONE', #15834, #6885 ) ;
#13893 = CARTESIAN_POINT ( 'NONE',  ( -28.99999999999999645, 29.50000000000000000, -27.00000000000000000 ) ) ;
#13894 = CARTESIAN_POINT ( 'NONE',  ( 7.937578510445358226, -3.514536757623690999, 12.49999999999999112 ) ) ;
#13895 = DIRECTION ( 'NONE',  ( -0.7071067811865660024, 0.000000000000000000, -0.7071067811865291430 ) ) ;
#13896 = CARTESIAN_POINT ( 'NONE',  ( 23.00000000000000000, 0.000000000000000000, 0.000000000000000000 ) ) ;
#13897 = DIRECTION ( 'NONE',  ( -0.000000000000000000, -0.000000000000000000, 1.000000000000000000 ) ) ;
#13898 = CARTESIAN_POINT ( 'NONE',  ( -40.50000000000000000, -51.00000000000000711, 0.5000000000000004441 ) ) ;
#13899 = EDGE_CURVE ( 'NONE', #22869, #3165, #16323, .T. ) ;
#13900 = VECTOR ( 'NONE', #2511, 999.9999999999998863 ) ;
#13901 = DIRECTION ( 'NONE',  ( 1.000000000000000000, 0.000000000000000000, 0.000000000000000000 ) ) ;
#13902 = CARTESIAN_POINT ( 'NONE',  ( 0.000000000000000000, 0.000000000000000000, 15.50000000000000000 ) ) ;
#13903 = LINE ( 'NONE', #21346, #16857 ) ;
#13904 = PRODUCT_DEFINITION_FORMATION_WITH_SPECIFIED_SOURCE ( 'ANY', '', #13079, .NOT_KNOWN. ) ;
#13905 = VECTOR ( 'NONE', #6774, 1000.000000000000000 ) ;
#13906 = DIRECTION ( 'NONE',  ( 0.000000000000000000, -1.000000000000000000, 0.000000000000000000 ) ) ;
#13907 = EDGE_CURVE ( 'NONE', #17649, #16165, #10707, .T. ) ;
#13908 = ORIENTED_EDGE ( 'NONE', *, *, #8215, .F. ) ;
#13909 = CARTESIAN_POINT ( 'NONE',  ( -2.935661446562617183, 9.035036904803758873, -11.80674201446023375 ) ) ;
#13910 =( BOUNDED_CURVE ( )  B_SPLINE_CURVE ( 2, ( #21491, #4786, #19679, #11700, #6235, #13676, #757, #10001, #15609, #22112, #8655 ),
 .UNSPECIFIED., .F., .T. ) 
 B_SPLINE_CURVE_WITH_KNOTS ( ( 3, 2, 2, 2, 2, 3 ),
 ( 0.3000000000000000999, 0.3200000000000001177, 0.3400000000000000799, 0.3600000000000000422, 0.3800000000000000044, 0.4000000000000000222 ),
 .UNSPECIFIED. ) 
 CURVE ( )  GEOMETRIC_REPRESENTATION_ITEM ( )  RATIONAL_B_SPLINE_CURVE ( ( 0.9999999999999997780, 0.9510565162951537532, 1.000000000000000000, 0.9510565162951535312, 1.000000000000000000, 0.9510565162951535312, 1.000000000000000000, 0.9510565162951535312, 1.000000000000000000, 0.9510565162951535312, 1.000000000000000000 ) ) 
 REPRESENTATION_ITEM ( '' )  );
#13911 = ORIENTED_EDGE ( 'NONE', *, *, #18442, .T. ) ;
#13912 = CARTESIAN_POINT ( 'NONE',  ( 5.871322893124553133, -8.081182679343980269, 3.759589141758144404 ) ) ;
#13913 = FACE_OUTER_BOUND ( 'NONE', #20437, .T. ) ;
#13914 = ORIENTED_EDGE ( 'NONE', *, *, #6012, .F. ) ;
#13915 = SHAPE_REPRESENTATION_RELATIONSHIP ( 'NONE' , 'NONE' ,  #23741, #8998 ) ;
#13916 = LINE ( 'NONE', #485, #11054 ) ;
#13917 = CARTESIAN_POINT ( 'NONE',  ( -5.871322893124554021, 8.081182679343978492, 2.759589141758142627 ) ) ;
#13918 = CARTESIAN_POINT ( 'NONE',  ( 30.68762588338048403, 45.64284848299539732, -3.000000000000000000 ) ) ;
#13919 = AXIS2_PLACEMENT_3D ( 'NONE', #23807, #1247, #1600 ) ;
#13920 = DIRECTION ( 'NONE',  ( 0.000000000000000000, 0.000000000000000000, 1.000000000000000000 ) ) ;
#13921 = CARTESIAN_POINT ( 'NONE',  ( 9.000000000000000000, 1.102182119232617714E-15, 53.00000000000000000 ) ) ;
#13922 = LINE ( 'NONE', #6221, #9137 ) ;
#13923 = DIRECTION ( 'NONE',  ( -1.337728473353585242E-16, 1.000000000000000000, -0.000000000000000000 ) ) ;
#13924 = PRODUCT ( 'Sleeve', 'Sleeve', '', ( #11373 ) ) ;
#13925 = ORIENTED_EDGE ( 'NONE', *, *, #18409, .T. ) ;
#13926 = EDGE_LOOP ( 'NONE', ( #22080, #10594, #10055, #13995 ) ) ;
#13927 = CARTESIAN_POINT ( 'NONE',  ( 85.63636363636365445, -4.172000000000000597, 0.000000000000000000 ) ) ;
#13928 = CYLINDRICAL_SURFACE ( 'NONE', #9096, 1.500000000000002887 ) ;
#13929 = DIRECTION ( 'NONE',  ( -0.000000000000000000, -0.000000000000000000, -1.000000000000000000 ) ) ;
#13930 = CARTESIAN_POINT ( 'NONE',  ( 5.000000000000000000, 4.685197434473818312, -1.301042606982605321E-15 ) ) ;
#13931 = EDGE_CURVE ( 'NONE', #22311, #15047, #11526, .T. ) ;
#13932 = VERTEX_POINT ( 'NONE', #3518 ) ;
#13933 = EDGE_CURVE ( 'NONE', #3090, #13127, #8552, .T. ) ;
#13934 = LINE ( 'NONE', #14472, #14891 ) ;
#13935 = DIRECTION ( 'NONE',  ( -1.000000000000000000, 0.000000000000000000, 0.000000000000000000 ) ) ;
#13936 = ORIENTED_EDGE ( 'NONE', *, *, #5963, .T. ) ;
#13937 = CARTESIAN_POINT ( 'NONE',  ( 9.499999999999790390, 3.086737114213260025, -7.306742014460234635 ) ) ;
#13938 = ORIENTED_EDGE ( 'NONE', *, *, #17966, .F. ) ;
#13939 = CARTESIAN_POINT ( 'NONE',  ( -20.85000000000000853, 15.04000000000000092, 25.00000000000000000 ) ) ;
#13940 = CARTESIAN_POINT ( 'NONE',  ( -2.682529543899159208, -8.255977015246598327, 10.03316557810918930 ) ) ;
#13941 = DIRECTION ( 'NONE',  ( -1.000000000000000000, -0.000000000000000000, -0.000000000000000000 ) ) ;
#13942 = DIRECTION ( 'NONE',  ( 0.000000000000000000, 0.000000000000000000, -1.000000000000000000 ) ) ;
#13943 = CARTESIAN_POINT ( 'NONE',  ( 34.10000000000000853, 29.50000000000000000, 27.00000000000000000 ) ) ;
#13944 = CARTESIAN_POINT ( 'NONE',  ( 40.00000000000000000, -28.80990663662251450, 11.00000000000000000 ) ) ;
#13945 = EDGE_LOOP ( 'NONE', ( #9261, #441, #2624, #21941 ) ) ;
#13946 = VERTEX_POINT ( 'NONE', #6863 ) ;
#13947 = DIRECTION ( 'NONE',  ( -0.000000000000000000, -0.000000000000000000, 1.000000000000000000 ) ) ;
#13948 = VECTOR ( 'NONE', #3196, 1000.000000000000000 ) ;
#13949 = EDGE_CURVE ( 'NONE', #6921, #2673, #16604, .T. ) ;
#13950 = CARTESIAN_POINT ( 'NONE',  ( -9.500000000000000000, -6.482511860946779655E-13, -8.206742014460234103 ) ) ;
#13951 = ORIENTED_EDGE ( 'NONE', *, *, #6251, .F. ) ;
#13952 = DIRECTION ( 'NONE',  ( 0.5735764363510424957, 0.8191520442889943521, 0.000000000000000000 ) ) ;
#13953 = ORIENTED_EDGE ( 'NONE', *, *, #7110, .T. ) ;
#13954 = EDGE_CURVE ( 'NONE', #17382, #6547, #14053, .T. ) ;
#13955 = EDGE_CURVE ( 'NONE', #2457, #14126, #4801, .T. ) ;
#13956 = VERTEX_POINT ( 'NONE', #15762 ) ;
#13957 = CARTESIAN_POINT ( 'NONE',  ( 41.00000000000000000, 5.999999999999986677, 11.00000000000000000 ) ) ;
#13958 = EDGE_CURVE ( 'NONE', #13716, #21260, #24022, .T. ) ;
#13959 = DIRECTION ( 'NONE',  ( 0.000000000000000000, -1.000000000000000000, 0.000000000000000000 ) ) ;
#13960 = ADVANCED_FACE ( 'NONE', ( #4672 ), #2191, .T. ) ;
#13961 = DIRECTION ( 'NONE',  ( -1.000000000000000000, -1.224606353822377258E-16, -0.000000000000000000 ) ) ;
#13962 = LINE ( 'NONE', #6640, #7960 ) ;
#13963 = VERTEX_POINT ( 'NONE', #23223 ) ;
#13964 = CARTESIAN_POINT ( 'NONE',  ( -40.00000000000000000, 0.000000000000000000, 12.00000000000000000 ) ) ;
#13965 = DIRECTION ( 'NONE',  ( -1.000000000000000000, -1.224606353822377258E-16, -0.000000000000000000 ) ) ;
#13966 = DIRECTION ( 'NONE',  ( 0.000000000000000000, 0.000000000000000000, 1.000000000000000000 ) ) ;
#13967 = EDGE_LOOP ( 'NONE', ( #9028, #23986, #21594, #16065 ) ) ;
#13968 = VECTOR ( 'NONE', #16899, 1000.000000000000000 ) ;
#13969 = CARTESIAN_POINT ( 'NONE',  ( -7.685661446562381371, 5.583959896777970222, 4.859589141758143604 ) ) ;
#13970 = VERTEX_POINT ( 'NONE', #6508 ) ;
#13971 = ORIENTED_EDGE ( 'NONE', *, *, #13409, .F. ) ;
#13972 = VERTEX_POINT ( 'NONE', #12077 ) ;
#13973 = ORIENTED_EDGE ( 'NONE', *, *, #6689, .F. ) ;
#13974 = CARTESIAN_POINT ( 'NONE',  ( 42.00000000000000000, 25.22443390181681622, -3.000000000000000000 ) ) ;
#13975 = AXIS2_PLACEMENT_3D ( 'NONE', #13518, #23292, #9823 ) ;
#13976 = EDGE_CURVE ( 'NONE', #8087, #2345, #12705, .T. ) ;
#13977 = LINE ( 'NONE', #1056, #23881 ) ;
#13978 = ORIENTED_EDGE ( 'NONE', *, *, #10942, .F. ) ;
#13979 = CARTESIAN_POINT ( 'NONE',  ( -17.59008829125738060, -9.499485695642615468, 0.4958780962348248722 ) ) ;
#13980 = DIRECTION ( 'NONE',  ( 0.000000000000000000, 0.000000000000000000, 1.000000000000000000 ) ) ;
#13981 = ORIENTED_EDGE ( 'NONE', *, *, #2097, .F. ) ;
#13982 = CARTESIAN_POINT ( 'NONE',  ( 80.69295543108962931, -9.244463733058732095E-30, 5.000000000000007994 ) ) ;
#13983 = COLOUR_RGB ( '',0.7921568627450980005, 0.8196078431372548767, 0.9333333333333333481 ) ;
#13985 = EDGE_CURVE ( 'NONE', #14530, #23937, #11313, .T. ) ;
#13984 = DIRECTION ( 'NONE',  ( -0.000000000000000000, -0.000000000000000000, -1.000000000000000000 ) ) ;
#13986 = CARTESIAN_POINT ( 'NONE',  ( -2.935661446562617183, 9.035036904803758873, 5.806742014460233747 ) ) ;
#13987 = LINE ( 'NONE', #13735, #3501 ) ;
#13988 = ADVANCED_FACE ( 'NONE', ( #7907 ), #5750, .T. ) ;
#13989 = DIRECTION ( 'NONE',  ( -0.000000000000000000, -0.000000000000000000, -1.000000000000000000 ) ) ;
#13990 = DIRECTION ( 'NONE',  ( 0.000000000000000000, -1.000000000000000000, 0.000000000000000000 ) ) ;
#13991 = CARTESIAN_POINT ( 'NONE',  ( 0.000000000000000000, 0.000000000000000000, -2.500000000000000000 ) ) ;
#13992 = DIRECTION ( 'NONE',  ( -1.000000000000000000, -0.000000000000000000, -0.000000000000000000 ) ) ;
#13993 = CARTESIAN_POINT ( 'NONE',  ( 8.680847955711007202, 5.912916378492122225E-13, -10.63316557810918894 ) ) ;
#13994 = DIRECTION ( 'NONE',  ( 0.000000000000000000, -1.000000000000000000, 0.000000000000000000 ) ) ;
#13995 = ORIENTED_EDGE ( 'NONE', *, *, #13722, .F. ) ;
#13996 = EDGE_LOOP ( 'NONE', ( #20047, #16924, #19597, #12275, #11024 ) ) ;
#13997 = CARTESIAN_POINT ( 'NONE',  ( -1.504652183083727168, 9.499999999999904077, 3.757996296007079184 ) ) ;
#13998 = EDGE_LOOP ( 'NONE', ( #13856, #16786, #15846, #18989 ) ) ;
#13999 = DIRECTION ( 'NONE',  ( 0.000000000000000000, 0.000000000000000000, 1.000000000000000000 ) ) ;
#14000 = ORIENTED_EDGE ( 'NONE', *, *, #23057, .F. ) ;
#14001 = ORIENTED_EDGE ( 'NONE', *, *, #13087, .T. ) ;
#14002 = DIRECTION ( 'NONE',  ( -0.000000000000000000, -0.000000000000000000, -1.000000000000000000 ) ) ;
#14003 = DIRECTION ( 'NONE',  ( 1.000000000000000000, 0.000000000000000000, 0.000000000000000000 ) ) ;
#14004 = UNCERTAINTY_MEASURE_WITH_UNIT (LENGTH_MEASURE( 1.000000000000000082E-05 ), #10936, 'distance_accuracy_value', 'NONE');
#14005 = CARTESIAN_POINT ( 'NONE',  ( 20.85000000000000497, -15.04000000000000270, 2.200000000000000178 ) ) ;
#14006 = PLANE ( 'NONE',  #16579 ) ;
#14007 = CARTESIAN_POINT ( 'NONE',  ( 0.000000000000000000, 0.000000000000000000, 6.000000000000000000 ) ) ;
#14008 = EDGE_CURVE ( 'NONE', #14945, #21512, #12327, .T. ) ;
#14009 = VERTEX_POINT ( 'NONE', #15355 ) ;
#14010 = DIRECTION ( 'NONE',  ( -1.000000000000000000, -0.000000000000000000, -0.000000000000000000 ) ) ;
#14011 = DIRECTION ( 'NONE',  ( -1.000000000000000000, 0.000000000000000000, -0.000000000000000000 ) ) ;
#14012 = ORIENTED_EDGE ( 'NONE', *, *, #14215, .T. ) ;
#14013 = CYLINDRICAL_SURFACE ( 'NONE', #7838, 1.500000000000000000 ) ;
#14014 = EDGE_LOOP ( 'NONE', ( #5298, #7513 ) ) ;
#14015 = ADVANCED_FACE ( 'NONE', ( #4030 ), #9860, .T. ) ;
#14016 = DIRECTION ( 'NONE',  ( 0.000000000000000000, -6.938893903907222067E-15, 1.000000000000000000 ) ) ;
#14017 = CARTESIAN_POINT ( 'NONE',  ( 28.27483331787887977, 41.23752903419610760, 11.00000000000000000 ) ) ;
#14018 = DIRECTION ( 'NONE',  ( -0.000000000000000000, -0.000000000000000000, -1.000000000000000000 ) ) ;
#14019 = VERTEX_POINT ( 'NONE', #22572 ) ;
#14020 = CARTESIAN_POINT ( 'NONE',  ( -5.622572944242076564E-13, 8.680847955711007202, -3.133165578109187166 ) ) ;
#14021 = ORIENTED_EDGE ( 'NONE', *, *, #20354, .F. ) ;
#14022 = ORIENTED_EDGE ( 'NONE', *, *, #14449, .T. ) ;
#14023 = CARTESIAN_POINT ( 'NONE',  ( -9.500000000000000000, -6.482511860946779655E-13, 3.059589141758143338 ) ) ;
#14024 = DIRECTION ( 'NONE',  ( 0.000000000000000000, 0.000000000000000000, 1.000000000000000000 ) ) ;
#14025 = ORIENTED_EDGE ( 'NONE', *, *, #21481, .T. ) ;
#14026 = CIRCLE ( 'NONE', #13220, 14.99999999999999822 ) ;
#14027 = AXIS2_PLACEMENT_3D ( 'NONE', #1537, #8950, #16393 ) ;
#14028 = DIRECTION ( 'NONE',  ( 0.5000000000000002220, -0.8660254037844384856, 0.000000000000000000 ) ) ;
#14029 = CARTESIAN_POINT ( 'NONE',  ( -2.352265130537441795, -9.224593858590012019, 3.479461880036843535 ) ) ;
#14030 = EDGE_CURVE ( 'NONE', #14101, #6887, #9367, .T. ) ;
#14031 = EDGE_LOOP ( 'NONE', ( #7331, #17433, #12346, #2807 ) ) ;
#14032 = CARTESIAN_POINT ( 'NONE',  ( 4.489900896931573904, 0.000000000000000000, -8.500000000000000000 ) ) ;
#14033 = PLANE ( 'NONE',  #18953 ) ;
#14034 = DIRECTION ( 'NONE',  ( -1.000000000000000000, -1.224606353822377258E-16, -0.000000000000000000 ) ) ;
#14035 = ADVANCED_FACE ( 'NONE', ( #5856 ), #14278, .T. ) ;
#14036 = DIRECTION ( 'NONE',  ( -1.000000000000000000, 0.000000000000000000, 0.000000000000000000 ) ) ;
#14037 = ORIENTED_EDGE ( 'NONE', *, *, #2291, .F. ) ;
#14038 = CARTESIAN_POINT ( 'NONE',  ( 41.73082370883257397, -27.62204025492843940, -1.500000000000000000 ) ) ;
#14039 = EDGE_CURVE ( 'NONE', #17649, #3750, #6892, .T. ) ;
#14040 = ORIENTED_EDGE ( 'NONE', *, *, #13715, .T. ) ;
#14041 = LINE ( 'NONE', #12192, #16405 ) ;
#14042 = DIRECTION ( 'NONE',  ( 1.000000000000000000, 0.000000000000000000, 0.000000000000000000 ) ) ;
#14043 = CARTESIAN_POINT ( 'NONE',  ( 58.00000000000000000, 4.172000000000015696, 0.000000000000000000 ) ) ;
#14044 = FACE_OUTER_BOUND ( 'NONE', #22170, .T. ) ;
#14045 = CARTESIAN_POINT ( 'NONE',  ( -36.00000000000001421, 50.99999999999999289, 0.5000000000000004441 ) ) ;
#14046 = ORIENTED_EDGE ( 'NONE', *, *, #8035, .T. ) ;
#14047 = DIRECTION ( 'NONE',  ( 0.000000000000000000, 0.000000000000000000, 1.000000000000000000 ) ) ;
#14048 = VERTEX_POINT ( 'NONE', #17319 ) ;
#14049 = EDGE_LOOP ( 'NONE', ( #4068, #22740, #14001 ) ) ;
#14050 = CARTESIAN_POINT ( 'NONE',  ( 2.682529543899157876, 8.255977015246598327, 5.033165578109189298 ) ) ;
#14051 = CARTESIAN_POINT ( 'NONE',  ( 68.76159002345582394, 7.562528597612068045E-15, 0.000000000000000000 ) ) ;
#14052 = CARTESIAN_POINT ( 'NONE',  ( -41.99999999999997158, -25.22443390181683043, -1.500000000000000000 ) ) ;
#14053 = LINE ( 'NONE', #21751, #23255 ) ;
#14054 = DIRECTION ( 'NONE',  ( 0.000000000000000000, 0.000000000000000000, 1.000000000000000000 ) ) ;
#14056 = ORIENTED_EDGE ( 'NONE', *, *, #10656, .T. ) ;
#14055=STYLED_ITEM('',(#24169),#18256);
#14057 = EDGE_CURVE ( 'NONE', #21225, #3090, #17400, .T. ) ;
#14058 = ORIENTED_EDGE ( 'NONE', *, *, #18494, .T. ) ;
#14059 = LINE ( 'NONE', #21507, #6865 ) ;
#14060 = EDGE_CURVE ( 'NONE', #18444, #13696, #14674, .T. ) ;
#14061 = CARTESIAN_POINT ( 'NONE',  ( 7.685661446561619314, 5.583959896779020049, -7.406742014460233392 ) ) ;
#14062 = ORIENTED_EDGE ( 'NONE', *, *, #23862, .T. ) ;
#14063 = ORIENTED_EDGE ( 'NONE', *, *, #22469, .T. ) ;
#14064 = CARTESIAN_POINT ( 'NONE',  ( -7.037334108778454222, -6.010000779825212192, -12.25356292181664131 ) ) ;
#14065 = DIRECTION ( 'NONE',  ( 1.000000000000000000, 0.000000000000000000, 0.000000000000000000 ) ) ;
#14066 = EDGE_LOOP ( 'NONE', ( #6125, #4333, #9436, #10114 ) ) ;
#14067 = CARTESIAN_POINT ( 'NONE',  ( 10.00000000000000000, 0.000000000000000000, 0.000000000000000000 ) ) ;
#14068 = VERTEX_POINT ( 'NONE', #9622 ) ;
#14069 = DIRECTION ( 'NONE',  ( -1.000000000000000000, -1.224606353822377258E-16, -0.000000000000000000 ) ) ;
#14070 = DIRECTION ( 'NONE',  ( 1.000000000000000000, 0.000000000000000000, 0.000000000000000000 ) ) ;
#14071 = DIRECTION ( 'NONE',  ( -1.000000000000000000, 0.000000000000000000, 0.000000000000000000 ) ) ;
#14072 = DIRECTION ( 'NONE',  ( -0.5654966663575777819, -0.8247505806839220410, 0.000000000000000000 ) ) ;
#14073 = DIRECTION ( 'NONE',  ( 1.000000000000000000, 0.000000000000000000, -0.000000000000000000 ) ) ;
#14074 = VERTEX_POINT ( 'NONE', #17070 ) ;
#14075 = CYLINDRICAL_SURFACE ( 'NONE', #15332, 3.000000000000002665 ) ;
#14076 = CARTESIAN_POINT ( 'NONE',  ( 4.489900896931573904, 0.000000000000000000, 0.000000000000000000 ) ) ;
#14077 = DIRECTION ( 'NONE',  ( -1.000000000000000000, -0.000000000000000000, 0.000000000000000000 ) ) ;
#14078 = MECHANICAL_DESIGN_GEOMETRIC_PRESENTATION_REPRESENTATION (  '', ( #2793 ), #17175 ) ;
#14079 = CARTESIAN_POINT ( 'NONE',  ( 7.685661446562381371, -5.583959896777971110, 9.859589141758144493 ) ) ;
#14080 = ADVANCED_FACE ( 'NONE', ( #4279 ), #5334, .F. ) ;
#14081 = EDGE_CURVE ( 'NONE', #21962, #15898, #2952, .T. ) ;
#14082 = ORIENTED_EDGE ( 'NONE', *, *, #11736, .T. ) ;
#14083 = ORIENTED_EDGE ( 'NONE', *, *, #18660, .F. ) ;
#14084 = EDGE_CURVE ( 'NONE', #13109, #14877, #11546, .T. ) ;
#14085 = DIRECTION ( 'NONE',  ( -1.000000000000000000, -0.000000000000000000, -0.000000000000000000 ) ) ;
#14086 = EDGE_CURVE ( 'NONE', #19209, #4885, #22823, .T. ) ;
#14087 = DIRECTION ( 'NONE',  ( 1.000000000000000000, 0.000000000000000000, 0.000000000000000000 ) ) ;
#14088 = CARTESIAN_POINT ( 'NONE',  ( 40.00000000000000711, 29.50000000000000000, -27.00000000000000000 ) ) ;
#14089 = AXIS2_PLACEMENT_3D ( 'NONE', #7219, #10967, #18447 ) ;
#14090 = CARTESIAN_POINT ( 'NONE',  ( 0.000000000000000000, 0.000000000000000000, 12.50000000000000000 ) ) ;
#14091 = CIRCLE ( 'NONE', #22281, 8.000000000000021316 ) ;
#14092 = DIRECTION ( 'NONE',  ( 0.000000000000000000, 0.000000000000000000, -1.000000000000000000 ) ) ;
#14093 = CARTESIAN_POINT ( 'NONE',  ( -28.00000000000000355, -3.851859888774471706E-31, 11.00000000000000000 ) ) ;
#14094 = CARTESIAN_POINT ( 'NONE',  ( 6.809999908187194197E-13, -9.988891130263535700, 4.706742014460233214 ) ) ;
#14095 = DIRECTION ( 'NONE',  ( -0.000000000000000000, -0.000000000000000000, 1.000000000000000000 ) ) ;
#14096 = CARTESIAN_POINT ( 'NONE',  ( 2.570122167802765922, 0.000000000000000000, 9.725923461386811297 ) ) ;
#14097 = DIRECTION ( 'NONE',  ( -1.000000000000000000, -1.224606353822377258E-16, -0.000000000000000000 ) ) ;
#14098 = CYLINDRICAL_SURFACE ( 'NONE', #4894, 9.500000000000000000 ) ;
#14099 = CARTESIAN_POINT ( 'NONE',  ( 8.680847955710813579, 2.820578480814259326, -10.73316557810918681 ) ) ;
#14100 = EDGE_CURVE ( 'NONE', #16483, #18348, #13547, .T. ) ;
#14101 = VERTEX_POINT ( 'NONE', #4766 ) ;
#14102 = LINE ( 'NONE', #21562, #10539 ) ;
#14103 = EDGE_CURVE ( 'NONE', #10649, #12142, #1225, .T. ) ;
#14104 = ORIENTED_EDGE ( 'NONE', *, *, #1640, .F. ) ;
#14105 = AXIS2_PLACEMENT_3D ( 'NONE', #23305, #19639, #6320 ) ;
#14106 = CARTESIAN_POINT ( 'NONE',  ( -35.99999999999994316, -60.00000000000000000, 12.50000000000000000 ) ) ;
#14107 = PRODUCT_DEFINITION_SHAPE ( 'NONE', 'NONE',  #24115 ) ;
#14108 = CIRCLE ( 'NONE', #102, 4.172000000000008590 ) ;
#14109 = ORIENTED_EDGE ( 'NONE', *, *, #18500, .F. ) ;
#14110 = DIRECTION ( 'NONE',  ( -1.000000000000000000, -1.224606353822377258E-16, -0.000000000000000000 ) ) ;
#14111 = ORIENTED_EDGE ( 'NONE', *, *, #12106, .T. ) ;
#14112 = ORIENTED_EDGE ( 'NONE', *, *, #1604, .T. ) ;
#14113 = EDGE_CURVE ( 'NONE', #4922, #3497, #2801, .T. ) ;
#14114 = CARTESIAN_POINT ( 'NONE',  ( 0.000000000000000000, 0.000000000000000000, 0.2999999999999990452 ) ) ;
#14115 = CARTESIAN_POINT ( 'NONE',  ( 2.935661446561383503, 9.035036904804158553, -4.459589141758144137 ) ) ;
#14116 = EDGE_CURVE ( 'NONE', #17727, #910, #7641, .T. ) ;
#14117 = CARTESIAN_POINT ( 'NONE',  ( -1.847098821903592869, 8.812944685114501908, 101.3956069432029210 ) ) ;
#14118 = LINE ( 'NONE', #8244, #16211 ) ;
#14119 = DIRECTION ( 'NONE',  ( -1.000000000000000000, -0.000000000000000000, 0.000000000000000000 ) ) ;
#14120 = PLANE ( 'NONE',  #16832 ) ;
#14121 = VECTOR ( 'NONE', #8756, 1000.000000000000000 ) ;
#14122 = CIRCLE ( 'NONE', #16445, 8.500000000000000000 ) ;
#14123 = LINE ( 'NONE', #10566, #12645 ) ;
#14124 = VECTOR ( 'NONE', #2183, 1000.000000000000000 ) ;
#14125 = DIRECTION ( 'NONE',  ( 0.000000000000000000, -1.000000000000000000, 0.000000000000000000 ) ) ;
#14126 = VERTEX_POINT ( 'NONE', #8272 ) ;
#14127 = CARTESIAN_POINT ( 'NONE',  ( 0.000000000000000000, 0.000000000000000000, 4.000000000000000000 ) ) ;
#14128 = DIRECTION ( 'NONE',  ( -1.000000000000000000, 0.000000000000000000, 0.000000000000000000 ) ) ;
#14129 = AXIS2_PLACEMENT_3D ( 'NONE', #2355, #19082, #7955 ) ;
#14130 = CARTESIAN_POINT ( 'NONE',  ( 0.000000000000000000, 0.000000000000000000, 53.00000000000000000 ) ) ;
#14131 = ORIENTED_EDGE ( 'NONE', *, *, #7725, .F. ) ;
#14132 = CARTESIAN_POINT ( 'NONE',  ( -5.365059087799947335, 7.384370330706355290, -3.333165578109187344 ) ) ;
#14133 = EDGE_LOOP ( 'NONE', ( #826, #14063, #5524, #5249 ) ) ;
#14134 = ORIENTED_EDGE ( 'NONE', *, *, #2269, .T. ) ;
#14135 = CARTESIAN_POINT ( 'NONE',  ( -9.500000000000211386, 3.086737114211961064, 6.959589141758143249 ) ) ;
#14136 = CARTESIAN_POINT ( 'NONE',  ( -5.871322893123450015, -8.081182679344781405, 4.506742014460231260 ) ) ;
#14137 = VERTEX_POINT ( 'NONE', #16087 ) ;
#14138 = DIRECTION ( 'NONE',  ( -1.000000000000000000, 0.000000000000000000, 0.000000000000000000 ) ) ;
#14139 = AXIS2_PLACEMENT_3D ( 'NONE', #10911, #13920, #22423 ) ;
#14140 = CIRCLE ( 'NONE', #22341, 2.024999999999999911 ) ;
#14141 = EDGE_CURVE ( 'NONE', #13651, #23135, #18971, .T. ) ;
#14142 = AXIS2_PLACEMENT_3D ( 'NONE', #23074, #15237, #19061 ) ;
#14143 = ORIENTED_EDGE ( 'NONE', *, *, #15418, .F. ) ;
#14144 = EDGE_CURVE ( 'NONE', #20735, #20174, #2205, .T. ) ;
#14145 = AXIS2_PLACEMENT_3D ( 'NONE', #2312, #9725, #8142 ) ;
#14146 = PRESENTATION_STYLE_ASSIGNMENT (( #6712 ) ) ;
#14147 = DIRECTION ( 'NONE',  ( -0.000000000000000000, -0.000000000000000000, -1.000000000000000000 ) ) ;
#14148 = CONICAL_SURFACE ( 'NONE', #22328, 5.000000000000007994, 0.9599310885968855844 ) ;
#14149 = ORIENTED_EDGE ( 'NONE', *, *, #15548, .T. ) ;
#14150 = DIRECTION ( 'NONE',  ( -0.000000000000000000, -0.000000000000000000, -1.000000000000000000 ) ) ;
#14151 = VERTEX_POINT ( 'NONE', #13785 ) ;
#14152 = SPHERICAL_SURFACE ( 'NONE', #12500, 1.000000000000000000 ) ;
#14153 =( LENGTH_UNIT ( ) NAMED_UNIT ( * ) SI_UNIT ( .MILLI., .METRE. ) );
#14154 = DIRECTION ( 'NONE',  ( -0.000000000000000000, 0.000000000000000000, 1.000000000000000000 ) ) ;
#14155 = AXIS2_PLACEMENT_3D ( 'NONE', #23631, #12123, #12258 ) ;
#14156 = DIRECTION ( 'NONE',  ( 0.000000000000000000, -1.000000000000000000, 0.000000000000000000 ) ) ;
#14157 = ORIENTED_EDGE ( 'NONE', *, *, #7649, .T. ) ;
#14158 = EDGE_CURVE ( 'NONE', #8325, #13274, #22109, .T. ) ;
#14159 = AXIS2_PLACEMENT_3D ( 'NONE', #5405, #9169, #23605 ) ;
#14160 = CARTESIAN_POINT ( 'NONE',  ( 57.42022815836235594, -9.244463733058732095E-30, 5.000000000000007994 ) ) ;
#14161 = AXIS2_PLACEMENT_3D ( 'NONE', #19006, #13013, #226 ) ;
#14162 = ORIENTED_EDGE ( 'NONE', *, *, #20076, .T. ) ;
#14163 = CARTESIAN_POINT ( 'NONE',  ( -5.871322893124554021, 8.081182679343978492, -6.759589141758143072 ) ) ;
#14164 = ORIENTED_EDGE ( 'NONE', *, *, #15393, .T. ) ;
#14165 = AXIS2_PLACEMENT_3D ( 'NONE', #14780, #22134, #11326 ) ;
#14166 = ADVANCED_FACE ( 'NONE', ( #6595 ), #19521, .F. ) ;
#14167 = CARTESIAN_POINT ( 'NONE',  ( -1.374911245008260785, 8.680847955710920161, 3.184419859656034468 ) ) ;
#14168 = FACE_BOUND ( 'NONE', #11610, .T. ) ;
#14169 = ADVANCED_FACE ( 'NONE', ( #21473 ), #14622, .F. ) ;
#14170 = LINE ( 'NONE', #21628, #16068 ) ;
#14171 = EDGE_CURVE ( 'NONE', #21663, #5301, #10099, .T. ) ;
#14172 = DIRECTION ( 'NONE',  ( -0.000000000000000000, -0.000000000000000000, 1.000000000000000000 ) ) ;
#14173 = ORIENTED_EDGE ( 'NONE', *, *, #17926, .T. ) ;
#14174 = CARTESIAN_POINT ( 'NONE',  ( 23.00000000000000000, 5.985147671565707483, 12.89120389306417103 ) ) ;
#14175 = CIRCLE ( 'NONE', #23548, 10.00000000000000533 ) ;
#14176 = CARTESIAN_POINT ( 'NONE',  ( -2.935661446561384391, -9.035036904804158553, -6.606742014460233570 ) ) ;
#14177 = CIRCLE ( 'NONE', #1327, 6.050000000006053646 ) ;
#14178 = AXIS2_PLACEMENT_3D ( 'NONE', #22012, #23479, #6758 ) ;
#14179 = AXIS2_PLACEMENT_3D ( 'NONE', #8127, #15570, #23033 ) ;
#14180 = ORIENTED_EDGE ( 'NONE', *, *, #23368, .F. ) ;
#14181 = ORIENTED_EDGE ( 'NONE', *, *, #2638, .F. ) ;
#14182 = CARTESIAN_POINT ( 'NONE',  ( 66.72727272727273373, 7.491529369508391930E-15, 0.000000000000000000 ) ) ;
#14183 = CARTESIAN_POINT ( 'NONE',  ( 10.00000000000000178, 0.000000000000000000, 8.000000000000000000 ) ) ;
#14184 = DIRECTION ( 'NONE',  ( 0.000000000000000000, 0.000000000000000000, -1.000000000000000000 ) ) ;
#14185 = DIRECTION ( 'NONE',  ( 0.000000000000000000, 0.000000000000000000, 1.000000000000000000 ) ) ;
#14186 = VERTEX_POINT ( 'NONE', #23190 ) ;
#14187 = CARTESIAN_POINT ( 'NONE',  ( -9.499999999999998224, 1.163414459189985485E-15, 3.499999999999999556 ) ) ;
#14188 = EDGE_CURVE ( 'NONE', #13710, #17379, #12177, .T. ) ;
#14189 = CARTESIAN_POINT ( 'NONE',  ( 1.999999999999996669, 45.00000000000000000, -8.673617379884035472E-16 ) ) ;
#14190 = DIRECTION ( 'NONE',  ( -0.000000000000000000, -0.000000000000000000, -1.000000000000000000 ) ) ;
#14191 = DIRECTION ( 'NONE',  ( -1.000000000000000000, 2.600433232233976523E-16, 0.000000000000000000 ) ) ;
#14192 = AXIS2_PLACEMENT_3D ( 'NONE', #15072, #13243, #22651 ) ;
#14193 = VERTEX_POINT ( 'NONE', #17440 ) ;
#14194 = AXIS2_PLACEMENT_3D ( 'NONE', #6167, #11387, #2143 ) ;
#14195 = ORIENTED_EDGE ( 'NONE', *, *, #6248, .T. ) ;
#14196 = CIRCLE ( 'NONE', #3311, 1.000000000000000222 ) ;
#14197 = VERTEX_POINT ( 'NONE', #19656 ) ;
#14198 = CARTESIAN_POINT ( 'NONE',  ( 40.66734255040735491, -26.56420859267090862, -3.000000000000000000 ) ) ;
#14199 = CARTESIAN_POINT ( 'NONE',  ( 0.000000000000000000, 0.000000000000000000, 27.00000000000000000 ) ) ;
#14200 = FACE_OUTER_BOUND ( 'NONE', #338, .T. ) ;
#14201 = ORIENTED_EDGE ( 'NONE', *, *, #1253, .F. ) ;
#14202 = CARTESIAN_POINT ( 'NONE',  ( -16.82499651802897489, -7.532250541895351148, -5.808290850931487448 ) ) ;
#14203 = CARTESIAN_POINT ( 'NONE',  ( 5.000000000000000000, -3.513898075855364844, -2.028749999999997389 ) ) ;
#14204 = ORIENTED_EDGE ( 'NONE', *, *, #4884, .T. ) ;
#14205 = DIRECTION ( 'NONE',  ( 0.000000000000000000, 0.000000000000000000, -1.000000000000000000 ) ) ;
#14206 = CARTESIAN_POINT ( 'NONE',  ( 0.000000000000000000, -45.00000000000000000, -26.97499999999999432 ) ) ;
#14207 = VECTOR ( 'NONE', #21237, 1000.000000000000000 ) ;
#14208 = EDGE_CURVE ( 'NONE', #19925, #19205, #13657, .T. ) ;
#14209 = CONICAL_SURFACE ( 'NONE', #3696, 9.000000000000000000, 0.7853981633974509435 ) ;
#14210 = CARTESIAN_POINT ( 'NONE',  ( 7.685661446562381371, -5.583959896777971110, 5.006742014460233037 ) ) ;
#14211 = B_SPLINE_CURVE_WITH_KNOTS ( 'NONE', 3,
 ( #1371, #12331, #16590, #23800, #12685, #7199, #21741, #5031 ),
 .UNSPECIFIED., .F., .F.,
 ( 4, 2, 2, 4 ),
 ( 2.602085213965210256E-18, 0.001946159586596642611, 0.002919239379894961964, 0.003892319173193281752 ),
 .UNSPECIFIED. ) ;
#14212 = CARTESIAN_POINT ( 'NONE',  ( -39.99999999999999289, -29.50000000000001066, -27.00000000000000000 ) ) ;
#14213 = CARTESIAN_POINT ( 'NONE',  ( -20.85000000000000853, 15.04000000000000092, -25.00000000000000000 ) ) ;
#14214 = AXIS2_PLACEMENT_3D ( 'NONE', #18446, #9162, #16610 ) ;
#14215 = EDGE_CURVE ( 'NONE', #23407, #23565, #2931, .T. ) ;
#14216 = CARTESIAN_POINT ( 'NONE',  ( 17.49232137458054837, -9.205685982891273156, 2.395442301836270715 ) ) ;
#14217 = AXIS2_PLACEMENT_3D ( 'NONE', #2963, #18211, #9156 ) ;
#14218 = CARTESIAN_POINT ( 'NONE',  ( -9.000000000000000000, 0.000000000000000000, 0.4999999999999970024 ) ) ;
#14219 = EDGE_CURVE ( 'NONE', #9321, #12610, #7275, .T. ) ;
#14220 = FACE_OUTER_BOUND ( 'NONE', #22976, .T. ) ;
#14221 = EDGE_CURVE ( 'NONE', #13484, #4194, #9164, .T. ) ;
#14222 = AXIS2_PLACEMENT_3D ( 'NONE', #23029, #15322, #4508 ) ;
#14223 = CARTESIAN_POINT ( 'NONE',  ( -42.00000000000000000, 5.000000000000002665, 8.500000000000000000 ) ) ;
#14224 = AXIS2_PLACEMENT_3D ( 'NONE', #12901, #3884, #20715 ) ;
#14225 = EDGE_LOOP ( 'NONE', ( #22338, #18117, #1942, #8500, #4440, #6654 ) ) ;
#14226 = CARTESIAN_POINT ( 'NONE',  ( -2.682529543900285862, 8.255977015246234174, 5.233165578109188587 ) ) ;
#14227 = DIRECTION ( 'NONE',  ( -5.551115123125782702E-17, 0.000000000000000000, -1.000000000000000000 ) ) ;
#14228 = LINE ( 'NONE', #3027, #5453 ) ;
#14229 = EDGE_LOOP ( 'NONE', ( #5412, #709, #15756 ) ) ;
#14230 = ORIENTED_EDGE ( 'NONE', *, *, #2464, .F. ) ;
#14231 = LINE ( 'NONE', #5086, #7206 ) ;
#14232 = CARTESIAN_POINT ( 'NONE',  ( -9.500000000000211386, 3.086737114211961064, -6.959589141758143249 ) ) ;
#14233 = AXIS2_PLACEMENT_3D ( 'NONE', #9397, #7701, #1634 ) ;
#14234 = AXIS2_PLACEMENT_3D ( 'NONE', #22123, #20272, #1383 ) ;
#14235 = CARTESIAN_POINT ( 'NONE',  ( -2.999999999999996447, 8.485281374238571317, 98.99999999999998579 ) ) ;
#14236 = LINE ( 'NONE', #7151, #8815 ) ;
#14237 = CARTESIAN_POINT ( 'NONE',  ( 2.000000000000000000, 0.000000000000000000, 0.4999999999999995559 ) ) ;
#14238 = AXIS2_PLACEMENT_3D ( 'NONE', #15546, #23012, #6287 ) ;
#14239 = AXIS2_PLACEMENT_3D ( 'NONE', #12201, #2817, #8298 ) ;
#14240 = CARTESIAN_POINT ( 'NONE',  ( 9.999999999999998224, 1.224646799147353059E-15, 15.50000000000000000 ) ) ;
#14241 = ADVANCED_FACE ( 'NONE', ( #4649 ), #8825, .F. ) ;
#14242 = CARTESIAN_POINT ( 'NONE',  ( 61.48886275072855057, 5.000000000000015099, 0.000000000000000000 ) ) ;
#14243 = CARTESIAN_POINT ( 'NONE',  ( -41.00000000000000000, 6.000000000000000888, 12.00000000000000000 ) ) ;
#14244 = VERTEX_POINT ( 'NONE', #15973 ) ;
#14245 = DIRECTION ( 'NONE',  ( 1.000000000000000000, 0.000000000000000000, -0.000000000000000000 ) ) ;
#14246 = DIRECTION ( 'NONE',  ( -0.000000000000000000, 0.8660254037844392627, 0.4999999999999989453 ) ) ;
#14247 = ADVANCED_FACE ( 'NONE', ( #23432 ), #21723, .F. ) ;
#14248 = DIRECTION ( 'NONE',  ( -0.000000000000000000, -0.000000000000000000, 1.000000000000000000 ) ) ;
#14249 = ADVANCED_FACE ( 'NONE', ( #10584 ), #23211, .T. ) ;
#14250 = EDGE_LOOP ( 'NONE', ( #9007, #7835, #7698, #9259 ) ) ;
#14251 = CARTESIAN_POINT ( 'NONE',  ( -6.233975306307046963E-13, 9.127583699786111282, -5.133165578109188054 ) ) ;
#14252 = EDGE_CURVE ( 'NONE', #11063, #21535, #17002, .T. ) ;
#14253 =( GEOMETRIC_REPRESENTATION_CONTEXT ( 3 ) GLOBAL_UNCERTAINTY_ASSIGNED_CONTEXT ( ( #8126 ) ) GLOBAL_UNIT_ASSIGNED_CONTEXT ( ( #13162, #17183, #14864 ) ) REPRESENTATION_CONTEXT ( 'NONE', 'WORKASPACE' ) );
#14254 = EDGE_LOOP ( 'NONE', ( #4442, #18528 ) ) ;
#14255 = AXIS2_PLACEMENT_3D ( 'NONE', #17162, #14964, #11285 ) ;
#14256 = ORIENTED_EDGE ( 'NONE', *, *, #20810, .T. ) ;
#14257 = CARTESIAN_POINT ( 'NONE',  ( 7.685661446562381371, -5.583959896777971110, 13.00674201446023304 ) ) ;
#14258 = CARTESIAN_POINT ( 'NONE',  ( 7.685661446561619314, 5.583959896779020049, 7.406742014460233392 ) ) ;
#14259 = FACE_OUTER_BOUND ( 'NONE', #16674, .T. ) ;
#14260 = VECTOR ( 'NONE', #23554, 1000.000000000000000 ) ;
#14261 = VERTEX_POINT ( 'NONE', #6835 ) ;
#14262 = DIRECTION ( 'NONE',  ( 3.944304526105059027E-31, -2.465190328815661892E-32, 0.9999999999999997780 ) ) ;
#14263 = VECTOR ( 'NONE', #17985, 1000.000000000000000 ) ;
#14264 = FACE_OUTER_BOUND ( 'NONE', #14614, .T. ) ;
#14265 = DIRECTION ( 'NONE',  ( 0.000000000000000000, -1.000000000000000000, 0.000000000000000000 ) ) ;
#14266 = CARTESIAN_POINT ( 'NONE',  ( 40.99749999999998096, 5.618459588085056979E-15, -9.499999999999989342 ) ) ;
#14267 = CARTESIAN_POINT ( 'NONE',  ( -40.00000000000000000, -28.80990663662251450, 0.000000000000000000 ) ) ;
#14268 = DIRECTION ( 'NONE',  ( -1.000000000000000000, 0.000000000000000000, 0.000000000000000000 ) ) ;
#14269 = AXIS2_PLACEMENT_3D ( 'NONE', #21453, #4745, #9959 ) ;
#14270 = AXIS2_PLACEMENT_3D ( 'NONE', #19380, #23159, #2286 ) ;
#14271 = CARTESIAN_POINT ( 'NONE',  ( 67.30704456891035647, 7.562528597612068045E-15, 0.000000000000000000 ) ) ;
#14272 = EDGE_CURVE ( 'NONE', #11408, #598, #4114, .T. ) ;
#14273 = ORIENTED_EDGE ( 'NONE', *, *, #16991, .T. ) ;
#14274 = CIRCLE ( 'NONE', #18194, 17.87500000001787726 ) ;
#14275 = DIRECTION ( 'NONE',  ( 0.000000000000000000, 0.000000000000000000, 1.000000000000000000 ) ) ;
#14276 = PLANE ( 'NONE',  #7516 ) ;
#14277 = CARTESIAN_POINT ( 'NONE',  ( -7.152444901921760412, 6.260001551030978995, -3.501211579454638123 ) ) ;
#14278 = CONICAL_SURFACE ( 'NONE', #3767, 4.172000000000008590, 0.9599310885968742602 ) ;
#14279 = DIRECTION ( 'NONE',  ( -0.000000000000000000, -0.000000000000000000, -1.000000000000000000 ) ) ;
#14280 = EDGE_LOOP ( 'NONE', ( #4308, #15938, #22343, #4448, #16430 ) ) ;
#14281 = EDGE_CURVE ( 'NONE', #9356, #13857, #16436, .T. ) ;
#14282 = DIRECTION ( 'NONE',  ( -0.000000000000000000, -0.000000000000000000, -1.000000000000000000 ) ) ;
#14283 = ORIENTED_EDGE ( 'NONE', *, *, #7755, .T. ) ;
#14284 = CARTESIAN_POINT ( 'NONE',  ( 84.18181818181818699, 7.491529369508391930E-15, 0.000000000000000000 ) ) ;
#14285 = EDGE_LOOP ( 'NONE', ( #17558, #17207, #8686, #6594, #17878 ) ) ;
#14286 = CARTESIAN_POINT ( 'NONE',  ( -8.680847955711007202, -5.923547351154968927E-13, 5.633165578109188942 ) ) ;
#14287 = CIRCLE ( 'NONE', #6504, 5.000000000000007994 ) ;
#14288 = ORIENTED_EDGE ( 'NONE', *, *, #14442, .T. ) ;
#14289 = LINE ( 'NONE', #21984, #6515 ) ;
#14290 = DIRECTION ( 'NONE',  ( -0.9913301211009810654, -0.1313947906041722236, 0.000000000000000000 ) ) ;
#14291 = DIRECTION ( 'NONE',  ( 0.000000000000000000, 0.000000000000000000, 1.000000000000000000 ) ) ;
#14292 = ORIENTED_EDGE ( 'NONE', *, *, #69, .F. ) ;
#14293 = CARTESIAN_POINT ( 'NONE',  ( 42.00000000000000711, 26.82133436441677077, 11.58578643762690241 ) ) ;
#14294 = CARTESIAN_POINT ( 'NONE',  ( 57.42022815836235594, 5.000000000000016875, 6.123233995736777129E-16 ) ) ;
#14295 = CARTESIAN_POINT ( 'NONE',  ( -9.500000000000211386, 3.086737114211961064, -4.106742014460232681 ) ) ;
#14296 = VERTEX_POINT ( 'NONE', #12533 ) ;
#14297 = ORIENTED_EDGE ( 'NONE', *, *, #1801, .F. ) ;
#14298 = DIRECTION ( 'NONE',  ( -0.000000000000000000, -0.000000000000000000, -1.000000000000000000 ) ) ;
#14299 = EDGE_CURVE ( 'NONE', #10832, #2783, #3009, .T. ) ;
#14300 = DIRECTION ( 'NONE',  ( -1.000000000000000000, 0.000000000000000000, 0.000000000000000000 ) ) ;
#14301 = CARTESIAN_POINT ( 'NONE',  ( 27.99999999999998934, 50.99999999999999289, 0.5000000000000000000 ) ) ;
#14302 = ADVANCED_FACE ( 'NONE', ( #16569 ), #16224, .T. ) ;
#14303 = ORIENTED_EDGE ( 'NONE', *, *, #16361, .T. ) ;
#14304 = ADVANCED_FACE ( 'NONE', ( #18185 ), #17750, .F. ) ;
#14305 = PRODUCT_DEFINITION_SHAPE ( 'NONE', 'NONE',  #24110 ) ;
#14306 = DIRECTION ( 'NONE',  ( -1.000000000000000000, -1.224606353822377258E-16, -0.000000000000000000 ) ) ;
#14307 = VERTEX_POINT ( 'NONE', #20246 ) ;
#14308 = CARTESIAN_POINT ( 'NONE',  ( 75.45454545454545325, 7.491529369508391930E-15, 0.000000000000000000 ) ) ;
#14309 = DIRECTION ( 'NONE',  ( -1.000000000000000000, 0.000000000000000000, 0.000000000000000000 ) ) ;
#14310 = DIRECTION ( 'NONE',  ( 0.000000000000000000, 0.000000000000000000, -1.000000000000000000 ) ) ;
#14311 = LINE ( 'NONE', #19936, #17188 ) ;
#14312 = ORIENTED_EDGE ( 'NONE', *, *, #22907, .T. ) ;
#14313 = ORIENTED_EDGE ( 'NONE', *, *, #19437, .F. ) ;
#14314 = ORIENTED_EDGE ( 'NONE', *, *, #9846, .F. ) ;
#14315 = ORIENTED_EDGE ( 'NONE', *, *, #19388, .T. ) ;
#14316 = DIRECTION ( 'NONE',  ( -1.000000000000000000, 0.000000000000000000, -0.000000000000000000 ) ) ;
#14317 = ADVANCED_FACE ( 'NONE', ( #10713 ), #20090, .F. ) ;
#14318 = DIRECTION ( 'NONE',  ( 0.000000000000000000, -1.000000000000000000, 0.000000000000000000 ) ) ;
#14319 = DIRECTION ( 'NONE',  ( -0.000000000000000000, -0.000000000000000000, -1.000000000000000000 ) ) ;
#14320 = DIRECTION ( 'NONE',  ( 0.000000000000000000, 0.000000000000000000, 1.000000000000000000 ) ) ;
#14321 = ADVANCED_FACE ( 'NONE', ( #7180 ), #23275, .F. ) ;
#14322 = LINE ( 'NONE', #8944, #18979 ) ;
#14323 = EDGE_LOOP ( 'NONE', ( #4073, #12857 ) ) ;
#14324 = CARTESIAN_POINT ( 'NONE',  ( 41.00000000000000000, 5.999999999999986677, 10.49999999999999822 ) ) ;
#14325 = LINE ( 'NONE', #16963, #4832 ) ;
#14326 = FACE_OUTER_BOUND ( 'NONE', #18163, .T. ) ;
#14327 = ADVANCED_FACE ( 'NONE', ( #3285 ), #7297, .T. ) ;
#14328 = DIRECTION ( 'NONE',  ( -0.000000000000000000, -0.000000000000000000, -1.000000000000000000 ) ) ;
#14329 = DIRECTION ( 'NONE',  ( 1.000000000000000000, 0.000000000000000000, 0.000000000000000000 ) ) ;
#14330 = AXIS2_PLACEMENT_3D ( 'NONE', #12873, #3385, #5452 ) ;
#14331 = LINE ( 'NONE', #21794, #6315 ) ;
#14332 = CARTESIAN_POINT ( 'NONE',  ( 17.32314925601268740, -8.733074366907743524, 3.769949228126185048 ) ) ;
#14333 = AXIS2_PLACEMENT_3D ( 'NONE', #18352, #15037, #24083 ) ;
#14334 = CARTESIAN_POINT ( 'NONE',  ( 0.000000000000000000, 0.000000000000000000, 12.50000000000000000 ) ) ;
#14335 = CARTESIAN_POINT ( 'NONE',  ( 2.682529543900284974, -8.255977015246234174, -4.233165578109187699 ) ) ;
#14336 = ORIENTED_EDGE ( 'NONE', *, *, #5669, .F. ) ;
#14337 = CARTESIAN_POINT ( 'NONE',  ( 74.57977184163763695, 6.123233995736675563E-16, -5.000000000000007994 ) ) ;
#14338 = ORIENTED_EDGE ( 'NONE', *, *, #12476, .F. ) ;
#14339 = AXIS2_PLACEMENT_3D ( 'NONE', #15259, #410, #7460 ) ;
#14340 = DIRECTION ( 'NONE',  ( 1.000000000000000000, 0.000000000000000000, 0.000000000000000000 ) ) ;
#14341 = CARTESIAN_POINT ( 'NONE',  ( -31.74999999999995737, 9.797174393178825657E-16, -8.000000000000000000 ) ) ;
#14342 = ORIENTED_EDGE ( 'NONE', *, *, #6603, .F. ) ;
#14343 = EDGE_LOOP ( 'NONE', ( #19445, #17363 ) ) ;
#14344 = FACE_OUTER_BOUND ( 'NONE', #3863, .T. ) ;
#14345 = CARTESIAN_POINT ( 'NONE',  ( 9.500000000000000000, 6.470877716354879437E-13, -8.059589141758143782 ) ) ;
#14346 = AXIS2_PLACEMENT_3D ( 'NONE', #5284, #20531, #22357 ) ;
#14347 = CARTESIAN_POINT ( 'NONE',  ( -2.844896095177359197, 8.538902624151456067, 99.97216383474440704 ) ) ;
#14348 = DIRECTION ( 'NONE',  ( 0.000000000000000000, 0.000000000000000000, 1.000000000000000000 ) ) ;
#14349 = CYLINDRICAL_SURFACE ( 'NONE', #2158, 18.49999999999999645 ) ;
#14350 = EDGE_CURVE ( 'NONE', #22940, #22995, #2154, .T. ) ;
#14351 = EDGE_CURVE ( 'NONE', #16608, #17944, #5282, .T. ) ;
#14352 = CYLINDRICAL_SURFACE ( 'NONE', #1885, 9.500000000000000000 ) ;
#14353 = VERTEX_POINT ( 'NONE', #8490 ) ;
#14354 = CARTESIAN_POINT ( 'NONE',  ( -1.999999999999994449, -45.00000000000000000, 0.000000000000000000 ) ) ;
#14355 = CLOSED_SHELL ( 'NONE', ( #1205, #15482, #5078, #3816, #10521, #2912, #11407, #5747 ) ) ;
#14356 = ORIENTED_EDGE ( 'NONE', *, *, #22418, .T. ) ;
#14357 = LINE ( 'NONE', #3503, #3199 ) ;
#14358 = ORIENTED_EDGE ( 'NONE', *, *, #8919, .T. ) ;
#14359 = FACE_OUTER_BOUND ( 'NONE', #19088, .T. ) ;
#14360 = DIRECTION ( 'NONE',  ( -0.5735764363510519326, 0.8191520442889876907, 1.003171929053519816E-16 ) ) ;
#14361 = DIRECTION ( 'NONE',  ( 0.000000000000000000, -1.000000000000000000, 0.000000000000000000 ) ) ;
#14362 = CARTESIAN_POINT ( 'NONE',  ( -31.74999999999995737, 0.000000000000000000, 5.000000000000000888 ) ) ;
#14363 = VERTEX_POINT ( 'NONE', #940 ) ;
#14364 = CARTESIAN_POINT ( 'NONE',  ( 28.99999999999998579, -29.49999999999999645, -3.000000000000000000 ) ) ;
#14365 = CARTESIAN_POINT ( 'NONE',  ( -9.499999999999790390, -3.086737114213257804, -10.30674201446023375 ) ) ;
#14366 = CARTESIAN_POINT ( 'NONE',  ( 33.99999999999998579, -4.000000000000013323, 9.500000000000000000 ) ) ;
#14367 = ORIENTED_EDGE ( 'NONE', *, *, #21785, .F. ) ;
#14368 = EDGE_LOOP ( 'NONE', ( #18148, #8200, #6635, #5853 ) ) ;
#14369 = CARTESIAN_POINT ( 'NONE',  ( -6.822232771736903637E-13, 9.988891130263535700, 6.559589141758143782 ) ) ;
#14370 = CARTESIAN_POINT ( 'NONE',  ( -9.500000000000211386, 3.086737114211961064, 8.106742014460232681 ) ) ;
#14371 = DIRECTION ( 'NONE',  ( 1.000000000000000000, -0.000000000000000000, -0.000000000000000000 ) ) ;
#14372 = ORIENTED_EDGE ( 'NONE', *, *, #19934, .T. ) ;
#14373 = DIRECTION ( 'NONE',  ( 0.000000000000000000, 0.000000000000000000, 1.000000000000000000 ) ) ;
#14374 = EDGE_CURVE ( 'NONE', #6981, #19122, #10434, .T. ) ;
#14375 = CYLINDRICAL_SURFACE ( 'NONE', #7060, 9.499999999999994671 ) ;
#14376 = DIRECTION ( 'NONE',  ( -1.000000000000000000, 0.000000000000000000, 0.000000000000000000 ) ) ;
#14377 = LINE ( 'NONE', #18187, #8419 ) ;
#14378 = CIRCLE ( 'NONE', #17494, 4.999999999999997335 ) ;
#14379 = EDGE_CURVE ( 'NONE', #5307, #21442, #12117, .T. ) ;
#14380 =( NAMED_UNIT ( * ) SI_UNIT ( $, .STERADIAN. ) SOLID_ANGLE_UNIT ( ) );
#14381 = LINE ( 'NONE', #6480, #16466 ) ;
#14382 = EDGE_CURVE ( 'NONE', #19008, #4863, #22045, .T. ) ;
#14383 = EDGE_CURVE ( 'NONE', #2260, #6140, #813, .T. ) ;
#14384 = ORIENTED_EDGE ( 'NONE', *, *, #20335, .T. ) ;
#14385 = CONICAL_SURFACE ( 'NONE', #13208, 4.249999999999996447, 1.029744258676654090 ) ;
#14386 = CARTESIAN_POINT ( 'NONE',  ( 83.30704456891035647, -1.078520768856852078E-29, 5.000000000000007994 ) ) ;
#14387 = CARTESIAN_POINT ( 'NONE',  ( 0.000000000000000000, 0.000000000000000000, 0.000000000000000000 ) ) ;
#14388 = CARTESIAN_POINT ( 'NONE',  ( -2.983080266967717442, 45.00000000000000000, 3.000000000000002665 ) ) ;
#14389 = CARTESIAN_POINT ( 'NONE',  ( 35.99999999999999289, 50.99999999999999289, 0.000000000000000000 ) ) ;
#14390 = CARTESIAN_POINT ( 'NONE',  ( 43.50000000000002132, 50.99999999999998579, 0.000000000000000000 ) ) ;
#14391 = CARTESIAN_POINT ( 'NONE',  ( 8.680847955711007202, 5.912916378492122225E-13, -8.633165578109188942 ) ) ;
#14392 = DIRECTION ( 'NONE',  ( 0.000000000000000000, -1.000000000000000000, 0.000000000000000000 ) ) ;
#14393 = ORIENTED_EDGE ( 'NONE', *, *, #22476, .T. ) ;
#14394 = DIRECTION ( 'NONE',  ( -0.000000000000000000, 1.000000000000000000, 6.938893903907221278E-15 ) ) ;
#14395 = ORIENTED_EDGE ( 'NONE', *, *, #19579, .T. ) ;
#14396 = CIRCLE ( 'NONE', #20265, 11.68650000001168721 ) ;
#14397 = CARTESIAN_POINT ( 'NONE',  ( -8.680847955711200825, 2.820578480813073607, 5.533165578109187521 ) ) ;
#14398 = ORIENTED_EDGE ( 'NONE', *, *, #21024, .T. ) ;
#14399 = DIRECTION ( 'NONE',  ( -1.000000000000000000, 0.000000000000000000, 0.000000000000000000 ) ) ;
#14400 = EDGE_CURVE ( 'NONE', #598, #17838, #10729, .T. ) ;
#14401 = CYLINDRICAL_SURFACE ( 'NONE', #1657, 1.999999999999994449 ) ;
#14402 = CARTESIAN_POINT ( 'NONE',  ( 0.000000000000000000, -45.00000000000000000, 23.99999999999999645 ) ) ;
#14403 = DIRECTION ( 'NONE',  ( -0.7071067811865474617, 0.000000000000000000, -0.7071067811865474617 ) ) ;
#14404 = EDGE_CURVE ( 'NONE', #12988, #1921, #4852, .T. ) ;
#14405 = DIRECTION ( 'NONE',  ( 1.000000000000000000, 0.000000000000000000, 0.000000000000000000 ) ) ;
#14406 = EDGE_CURVE ( 'NONE', #15773, #23710, #5682, .T. ) ;
#14407 = EDGE_LOOP ( 'NONE', ( #11624, #18464, #20294, #23122 ) ) ;
#14408 = VERTEX_POINT ( 'NONE', #23396 ) ;
#14409 = DIRECTION ( 'NONE',  ( 0.000000000000000000, 0.000000000000000000, -1.000000000000000000 ) ) ;
#14410 = AXIS2_PLACEMENT_3D ( 'NONE', #7068, #16585, #3424 ) ;
#14411 = CYLINDRICAL_SURFACE ( 'NONE', #12905, 8.000000000000003553 ) ;
#14412 = FACE_OUTER_BOUND ( 'NONE', #7722, .T. ) ;
#14413 = EDGE_LOOP ( 'NONE', ( #21816, #15056, #12358, #5927, #15573 ) ) ;
#14414 = CARTESIAN_POINT ( 'NONE',  ( 59.45454545454545325, 7.491529369508391930E-15, 0.000000000000000000 ) ) ;
#14415 = CARTESIAN_POINT ( 'NONE',  ( 0.000000000000000000, 0.000000000000000000, 4.000000000000000000 ) ) ;
#14416 = ORIENTED_EDGE ( 'NONE', *, *, #19388, .F. ) ;
#14417 = DIRECTION ( 'NONE',  ( -1.000000000000000000, -0.000000000000000000, -0.000000000000000000 ) ) ;
#14418 = CARTESIAN_POINT ( 'NONE',  ( -40.89823313241237912, 26.41789760203348081, 27.00000000000000000 ) ) ;
#14419 = CARTESIAN_POINT ( 'NONE',  ( -7.685661446562381371, 5.583959896777970222, -4.006742014460233925 ) ) ;
#14420 = CARTESIAN_POINT ( 'NONE',  ( 6.809999908187194197E-13, -9.988891130263535700, 3.559589141758143338 ) ) ;
#14421 = CIRCLE ( 'NONE', #8964, 4.999999999999997335 ) ;
#14422 = VERTEX_POINT ( 'NONE', #15675 ) ;
#14423 = ORIENTED_EDGE ( 'NONE', *, *, #5570, .T. ) ;
#14424 = VERTEX_POINT ( 'NONE', #12128 ) ;
#14425 = ORIENTED_EDGE ( 'NONE', *, *, #14103, .F. ) ;
#14426 = CARTESIAN_POINT ( 'NONE',  ( 73.12522638709218370, 5.000000000000015099, 0.000000000000000000 ) ) ;
#14427 = EDGE_CURVE ( 'NONE', #12954, #6647, #19605, .T. ) ;
#14428 = CARTESIAN_POINT ( 'NONE',  ( 10.00000000000000178, 9.797174393178825657E-16, -8.000000000000000000 ) ) ;
#14429 = CARTESIAN_POINT ( 'NONE',  ( -39.99999999999999289, 15.50000000000000000, 12.50000000000000000 ) ) ;
#14430 = ORIENTED_EDGE ( 'NONE', *, *, #622, .F. ) ;
#14431 = CARTESIAN_POINT ( 'NONE',  ( 42.00000000000000000, 5.999999999999986677, 10.49999999999999822 ) ) ;
#14432 = ORIENTED_EDGE ( 'NONE', *, *, #4552, .T. ) ;
#14433 = CARTESIAN_POINT ( 'NONE',  ( 11.50000000000000000, -15.26463740537719005, -9.300885435430258141 ) ) ;
#14434 = CARTESIAN_POINT ( 'NONE',  ( 67.30704456891035647, 7.562528597612068045E-15, 0.000000000000000000 ) ) ;
#14435 = CARTESIAN_POINT ( 'NONE',  ( 23.00000000000000000, -9.374578970469563899, -10.68280860024325030 ) ) ;
#14436 = AXIS2_PLACEMENT_3D ( 'NONE', #2892, #8114, #4613 ) ;
#14437 = APPLICATION_CONTEXT ( 'automotive_design' ) ;
#14438 = DIRECTION ( 'NONE',  ( -0.000000000000000000, -0.000000000000000000, 1.000000000000000000 ) ) ;
#14439 = DIRECTION ( 'NONE',  ( -1.000000000000000000, 0.000000000000000000, 0.000000000000000000 ) ) ;
#14440 = DIRECTION ( 'NONE',  ( 0.000000000000000000, -0.000000000000000000, -1.000000000000000000 ) ) ;
#14441 = CARTESIAN_POINT ( 'NONE',  ( 8.680847955711199049, -2.820578480813074496, -4.533165578109188409 ) ) ;
#14442 = EDGE_CURVE ( 'NONE', #23460, #13598, #6618, .T. ) ;
#14443 = CARTESIAN_POINT ( 'NONE',  ( 5.000000000000000000, 2.342598717236902939, -4.057500000000001883 ) ) ;
#14444 = ORIENTED_EDGE ( 'NONE', *, *, #7056, .F. ) ;
#14445 = LINE ( 'NONE', #14808, #12113 ) ;
#14446 = ORIENTED_EDGE ( 'NONE', *, *, #4855, .T. ) ;
#14447 = EDGE_CURVE ( 'NONE', #3076, #16364, #9305, .T. ) ;
#14448 = CARTESIAN_POINT ( 'NONE',  ( 722.7818939062880190, 858.9837211537982284, 1368.981724745928204 ) ) ;
#14449 = EDGE_CURVE ( 'NONE', #10996, #20777, #22263, .T. ) ;
#14450 = DIRECTION ( 'NONE',  ( 1.000000000000000000, 0.000000000000000000, 0.000000000000000000 ) ) ;
#14451 = CIRCLE ( 'NONE', #19551, 9.000000000000001776 ) ;
#14452 = EDGE_LOOP ( 'NONE', ( #20373, #969, #17247 ) ) ;
#14453 = EDGE_LOOP ( 'NONE', ( #12497, #7624, #15650 ) ) ;
#14454 = EDGE_CURVE ( 'NONE', #3651, #15771, #3343, .T. ) ;
#14455 = FACE_OUTER_BOUND ( 'NONE', #21230, .T. ) ;
#14456 = CARTESIAN_POINT ( 'NONE',  ( 9.499999999999790390, 3.086737114213260025, -4.159589141758141650 ) ) ;
#14457 = VECTOR ( 'NONE', #15443, 1000.000000000000000 ) ;
#14458 = CARTESIAN_POINT ( 'NONE',  ( 76.03431729618309021, 7.562528597612068045E-15, 0.000000000000000000 ) ) ;
#14459 = DIRECTION ( 'NONE',  ( 0.000000000000000000, 0.9898214418809322401, 0.1423148382732887240 ) ) ;
#14460 = FACE_OUTER_BOUND ( 'NONE', #14529, .T. ) ;
#14461 = CARTESIAN_POINT ( 'NONE',  ( -29.00000000000000000, 29.49999999999999645, 11.50000000000000000 ) ) ;
#14462 = ORIENTED_EDGE ( 'NONE', *, *, #11157, .F. ) ;
#14463 = DIRECTION ( 'NONE',  ( 0.000000000000000000, -1.000000000000000000, 0.000000000000000000 ) ) ;
#14464 = ORIENTED_EDGE ( 'NONE', *, *, #15026, .T. ) ;
#14465 = LINE ( 'NONE', #8974, #5934 ) ;
#14466 = ORIENTED_EDGE ( 'NONE', *, *, #9930, .F. ) ;
#14467 = DIRECTION ( 'NONE',  ( -0.000000000000000000, -0.000000000000000000, -1.000000000000000000 ) ) ;
#14468 = DIRECTION ( 'NONE',  ( 0.000000000000000000, 0.4999999999999993339, -0.8660254037844390407 ) ) ;
#14469 = AXIS2_PLACEMENT_3D ( 'NONE', #22454, #2416, #5733 ) ;
#14470 = DIRECTION ( 'NONE',  ( -0.000000000000000000, -0.000000000000000000, -1.000000000000000000 ) ) ;
#14471 = EDGE_LOOP ( 'NONE', ( #10163, #20785, #6873, #14757 ) ) ;
#14472 = CARTESIAN_POINT ( 'NONE',  ( -42.00000000000000000, 26.82133436441678498, 11.00000000000000000 ) ) ;
#14473 = VECTOR ( 'NONE', #10780, 1000.000000000000000 ) ;
#14474 =( NAMED_UNIT ( * ) PLANE_ANGLE_UNIT ( ) SI_UNIT ( $, .RADIAN. ) );
#14475 = VERTEX_POINT ( 'NONE', #20312 ) ;
#14476 = ORIENTED_EDGE ( 'NONE', *, *, #11338, .F. ) ;
#14477 = CARTESIAN_POINT ( 'NONE',  ( -9.500000000000211386, 3.086737114211961064, 10.10674201446023446 ) ) ;
#14478 = ADVANCED_FACE ( 'NONE', ( #16287 ), #15003, .T. ) ;
#14479 = CARTESIAN_POINT ( 'NONE',  ( -5.871322893124554021, 8.081182679343978492, 9.906742014460235168 ) ) ;
#14480 = ORIENTED_EDGE ( 'NONE', *, *, #23224, .F. ) ;
#14481 = ADVANCED_FACE ( 'NONE', ( #23748 ), #5540, .F. ) ;
#14482 = ORIENTED_EDGE ( 'NONE', *, *, #21940, .T. ) ;
#14483 = CARTESIAN_POINT ( 'NONE',  ( 40.66734255040736201, -26.56420859267091217, -1.500000000000000000 ) ) ;
#14484 = DIRECTION ( 'NONE',  ( -1.000000000000000000, -1.224606353822377258E-16, -0.000000000000000000 ) ) ;
#14485 = FACE_BOUND ( 'NONE', #15207, .T. ) ;
#14486 = DIRECTION ( 'NONE',  ( -0.000000000000000000, -0.000000000000000000, -1.000000000000000000 ) ) ;
#14487 = VECTOR ( 'NONE', #16203, 1000.000000000000000 ) ;
#14488 = CONICAL_SURFACE ( 'NONE', #3981, 5.000000000000007994, 0.9599310885968855844 ) ;
#14489 = CARTESIAN_POINT ( 'NONE',  ( 82.14750088563508257, 7.420530141404717394E-15, 0.000000000000000000 ) ) ;
#14490 = DIRECTION ( 'NONE',  ( -1.000000000000000000, 0.000000000000000000, 0.000000000000000000 ) ) ;
#14491 = AXIS2_PLACEMENT_3D ( 'NONE', #15506, #5653, #9528 ) ;
#14492 = PRODUCT_DEFINITION_SHAPE ( 'NONE', 'NONE',  #12281 ) ;
#14493 = AXIS2_PLACEMENT_3D ( 'NONE', #17190, #8153, #19049 ) ;
#14494 = EDGE_LOOP ( 'NONE', ( #12278, #11215, #7779, #14367, #7172 ) ) ;
#14495 = AXIS2_PLACEMENT_3D ( 'NONE', #16369, #8823, #14309 ) ;
#14496 = CARTESIAN_POINT ( 'NONE',  ( 30.44534269664590553, -40.40463133211081015, 11.00000000000000000 ) ) ;
#14497 = ORIENTED_EDGE ( 'NONE', *, *, #2494, .T. ) ;
#14498 = DIRECTION ( 'NONE',  ( 0.000000000000000000, -0.5000000000000011102, -0.8660254037844380415 ) ) ;
#14499 = DIRECTION ( 'NONE',  ( 0.000000000000000000, 0.000000000000000000, -1.000000000000000000 ) ) ;
#14500 = FACE_OUTER_BOUND ( 'NONE', #18144, .T. ) ;
#14501 = CARTESIAN_POINT ( 'NONE',  ( 5.871322893124551356, -8.081182679343980269, -11.75958914175814485 ) ) ;
#14502 = CARTESIAN_POINT ( 'NONE',  ( 0.000000000000000000, 0.000000000000000000, -12.50000000000000000 ) ) ;
#14503 = CARTESIAN_POINT ( 'NONE',  ( 6.222797240145152671E-13, -9.127583699786111282, -8.133165578109188942 ) ) ;
#14504 = CARTESIAN_POINT ( 'NONE',  ( 40.66734255040738333, 26.56420859267091217, -1.500000000000000000 ) ) ;
#14505 = ORIENTED_EDGE ( 'NONE', *, *, #10272, .T. ) ;
#14506 = FACE_OUTER_BOUND ( 'NONE', #10748, .T. ) ;
#14507 = VERTEX_POINT ( 'NONE', #12973 ) ;
#14508 = CIRCLE ( 'NONE', #10223, 1.999999999999994449 ) ;
#14509 = CARTESIAN_POINT ( 'NONE',  ( 64.69295543108962931, 6.123233995736675563E-16, -5.000000000000007994 ) ) ;
#14510 = ADVANCED_FACE ( 'NONE', ( #11132 ), #5186, .T. ) ;
#14511 = AXIS2_PLACEMENT_3D ( 'NONE', #11444, #9621, #15216 ) ;
#14512 = CIRCLE ( 'NONE', #3219, 5.000000000000007994 ) ;
#14513 = LINE ( 'NONE', #3433, #256 ) ;
#14514 = EDGE_CURVE ( 'NONE', #10129, #14101, #20109, .T. ) ;
#14515 = AXIS2_PLACEMENT_3D ( 'NONE', #18760, #9602, #21306 ) ;
#14516 = ORIENTED_EDGE ( 'NONE', *, *, #17076, .F. ) ;
#14517 = FACE_BOUND ( 'NONE', #2795, .T. ) ;
#14518 = AXIS2_PLACEMENT_3D ( 'NONE', #14778, #16494, #20534 ) ;
#14519 = LINE ( 'NONE', #16471, #18098 ) ;
#14520 = DIRECTION ( 'NONE',  ( -0.000000000000000000, -0.000000000000000000, 1.000000000000000000 ) ) ;
#14521 = AXIS2_PLACEMENT_3D ( 'NONE', #14435, #17890, #8949 ) ;
#14522 = CARTESIAN_POINT ( 'NONE',  ( 0.000000000000000000, -45.00000000000000000, 0.000000000000000000 ) ) ;
#14523 = CIRCLE ( 'NONE', #19620, 49.00000000000000000 ) ;
#14524 =( BOUNDED_CURVE ( )  B_SPLINE_CURVE ( 2, ( #11109, #22014, #14419, #18462, #14784, #5165, #9052 ),
 .UNSPECIFIED., .F., .F. ) 
 B_SPLINE_CURVE_WITH_KNOTS ( ( 3, 2, 2, 3 ),
 ( 0.9000000000000000222, 0.9200000000000000400, 0.9399999999999999467, 0.9500000000000000666 ),
 .UNSPECIFIED. ) 
 CURVE ( )  GEOMETRIC_REPRESENTATION_ITEM ( )  RATIONAL_B_SPLINE_CURVE ( ( 1.000000000000000000, 0.9510565162951535312, 1.000000000000000000, 0.9510565162951535312, 1.000000000000000000, 0.9755282581475764880, 0.9755282581475768211 ) ) 
 REPRESENTATION_ITEM ( '' )  );
#14525 = CARTESIAN_POINT ( 'NONE',  ( 0.000000000000000000, 1.191082103573950341E-15, -9.725923461386811297 ) ) ;
#14526 = B_SPLINE_CURVE_WITH_KNOTS ( 'NONE', 3,
 ( #21869, #7218, #1508, #5279 ),
 .UNSPECIFIED., .F., .F.,
 ( 4, 4 ),
 ( 0.8197781486845410193, 1.000000000000000000 ),
 .UNSPECIFIED. ) ;
#14527 = FACE_OUTER_BOUND ( 'NONE', #3045, .T. ) ;
#14528 = CARTESIAN_POINT ( 'NONE',  ( 5.871322893123449127, 8.081182679344781405, -7.506742014460233037 ) ) ;
#14529 = EDGE_LOOP ( 'NONE', ( #696, #22355 ) ) ;
#14530 = VERTEX_POINT ( 'NONE', #7362 ) ;
#14531 = DIRECTION ( 'NONE',  ( -1.000000000000000000, -0.000000000000000000, -0.000000000000000000 ) ) ;
#14532 = CIRCLE ( 'NONE', #4020, 17.87500000001787726 ) ;
#14533 = AXIS2_PLACEMENT_3D ( 'NONE', #13372, #20340, #5815 ) ;
#14534 = CIRCLE ( 'NONE', #20378, 6.050000000006050982 ) ;
#14535 = DIRECTION ( 'NONE',  ( -1.000000000000000000, 0.000000000000000000, 0.000000000000000000 ) ) ;
#14536 = AXIS2_PLACEMENT_3D ( 'NONE', #20088, #5322, #3123 ) ;
#14537 = ADVANCED_FACE ( 'NONE', ( #20427 ), #3719, .T. ) ;
#14538 = AXIS2_PLACEMENT_3D ( 'NONE', #18692, #14669, #12827 ) ;
#14539 = ORIENTED_EDGE ( 'NONE', *, *, #155, .F. ) ;
#14540 = CIRCLE ( 'NONE', #20398, 9.499999999999996447 ) ;
#14541 = CARTESIAN_POINT ( 'NONE',  ( -40.99749999999999517, 0.000000000000000000, 0.000000000000000000 ) ) ;
#14542 = DIRECTION ( 'NONE',  ( -0.000000000000000000, 0.000000000000000000, -1.000000000000000000 ) ) ;
#14543 = VERTEX_POINT ( 'NONE', #9577 ) ;
#14544 = CARTESIAN_POINT ( 'NONE',  ( 5.000000000000000000, -2.342598717236916261, -4.057499999999997442 ) ) ;
#14545 = FACE_OUTER_BOUND ( 'NONE', #19476, .T. ) ;
#14546 = ADVANCED_FACE ( 'NONE', ( #19110 ), #21179, .F. ) ;
#14547 = LINE ( 'NONE', #16370, #3747 ) ;
#14548 = EDGE_CURVE ( 'NONE', #20316, #18527, #19321, .T. ) ;
#14549 = CYLINDRICAL_SURFACE ( 'NONE', #14836, 8.000000000000000000 ) ;
#14550 = AXIS2_PLACEMENT_3D ( 'NONE', #1709, #7190, #5734 ) ;
#14551 = EDGE_LOOP ( 'NONE', ( #3095, #8767, #20251, #9339 ) ) ;
#14552 = VECTOR ( 'NONE', #1742, 1000.000000000000000 ) ;
#14553 = AXIS2_PLACEMENT_3D ( 'NONE', #788, #13965, #8198 ) ;
#14554 = AXIS2_PLACEMENT_3D ( 'NONE', #11518, #9683, #1171 ) ;
#14555 = VERTEX_POINT ( 'NONE', #22644 ) ;
#14556 = DIRECTION ( 'NONE',  ( 1.000000000000000000, 0.000000000000000000, -0.000000000000000000 ) ) ;
#14557 = AXIS2_PLACEMENT_3D ( 'NONE', #3492, #1553, #7150 ) ;
#14558 = CYLINDRICAL_SURFACE ( 'NONE', #17251, 1.000000000000000888 ) ;
#14559 = ORIENTED_EDGE ( 'NONE', *, *, #4655, .T. ) ;
#14560 = CIRCLE ( 'NONE', #16139, 5.000000000000007994 ) ;
#14561 = VERTEX_POINT ( 'NONE', #17265 ) ;
#14562 = CARTESIAN_POINT ( 'NONE',  ( 5.000000000000000000, -3.755786496842893535E-15, -4.057500000000000107 ) ) ;
#14563 = ORIENTED_EDGE ( 'NONE', *, *, #13668, .F. ) ;
#14564 = DIRECTION ( 'NONE',  ( 1.000000000000000000, 0.000000000000000000, 0.000000000000000000 ) ) ;
#14565 = EDGE_CURVE ( 'NONE', #14193, #14261, #21272, .T. ) ;
#14566 = CARTESIAN_POINT ( 'NONE',  ( -8.778978273663913257, 3.506149232160788110, 12.05025702049722547 ) ) ;
#14567 = CARTESIAN_POINT ( 'NONE',  ( -2.935661446561384391, -9.035036904804158553, 10.60674201446023446 ) ) ;
#14568 = LINE ( 'NONE', #1539, #17611 ) ;
#14569 = CONICAL_SURFACE ( 'NONE', #20828, 1.999999999999994449, 1.029744258676653201 ) ;
#14570 = CARTESIAN_POINT ( 'NONE',  ( -31.74999999999995737, 6.123233995736767268E-16, -5.000000000000000888 ) ) ;
#14571 = CARTESIAN_POINT ( 'NONE',  ( -1.374911245008260785, 8.680847955710920161, -3.184419859656034468 ) ) ;
#14572 = CARTESIAN_POINT ( 'NONE',  ( 30.44534269664590553, 40.40463133211080304, 12.00000000000000000 ) ) ;
#14573 = AXIS2_PLACEMENT_3D ( 'NONE', #9191, #1641, #16642 ) ;
#14574 = ADVANCED_FACE ( 'NONE', ( #6058 ), #13498, .F. ) ;
#14575 = ADVANCED_FACE ( 'NONE', ( #2384 ), #9799, .T. ) ;
#14576 = ORIENTED_EDGE ( 'NONE', *, *, #7494, .F. ) ;
#14577 = DIRECTION ( 'NONE',  ( 0.000000000000000000, -1.000000000000000000, 0.000000000000000000 ) ) ;
#14578 = ORIENTED_EDGE ( 'NONE', *, *, #18033, .T. ) ;
#14579 = CIRCLE ( 'NONE', #17318, 5.000000000000007994 ) ;
#14580 = CONTEXT_DEPENDENT_SHAPE_REPRESENTATION ( #20238, #12354 ) ;
#14581 = CARTESIAN_POINT ( 'NONE',  ( 0.000000000000000000, 0.000000000000000000, 6.000000000000000000 ) ) ;
#14582 = ORIENTED_EDGE ( 'NONE', *, *, #12970, .F. ) ;
#14583 = ORIENTED_EDGE ( 'NONE', *, *, #8739, .T. ) ;
#14584 = CARTESIAN_POINT ( 'NONE',  ( -8.595784692538620320, 3.983312405694302782, -12.03999298932260409 ) ) ;
#14585 = CARTESIAN_POINT ( 'NONE',  ( -9.500000000000000000, -6.482511860946779655E-13, -5.059589141758143782 ) ) ;
#14586 = CONICAL_SURFACE ( 'NONE', #2921, 4.172000000000008590, 0.9599310885968742602 ) ;
#14587 = AXIS2_PLACEMENT_3D ( 'NONE', #9144, #14859, #22337 ) ;
#14588 = DIRECTION ( 'NONE',  ( -1.000000000000000000, -1.224606353822377258E-16, -0.000000000000000000 ) ) ;
#14589 = CARTESIAN_POINT ( 'NONE',  ( -5.622572944242077574E-13, 8.680847955711007202, 3.133165578109187610 ) ) ;
#14590 = LINE ( 'NONE', #5338, #13948 ) ;
#14591 = ADVANCED_FACE ( 'NONE', ( #13611 ), #4350, .F. ) ;
#14592 = AXIS2_PLACEMENT_3D ( 'NONE', #16781, #13012, #22908 ) ;
#14593 = CARTESIAN_POINT ( 'NONE',  ( -41.73082370883260239, 29.50000000000000711, 0.000000000000000000 ) ) ;
#14594 = ORIENTED_EDGE ( 'NONE', *, *, #10848, .T. ) ;
#14595 = DIRECTION ( 'NONE',  ( 0.000000000000000000, 0.000000000000000000, -1.000000000000000000 ) ) ;
#14596 = AXIS2_PLACEMENT_3D ( 'NONE', #15200, #21079, #17426 ) ;
#14597 = EDGE_CURVE ( 'NONE', #23003, #4197, #19734, .T. ) ;
#14598 = ORIENTED_EDGE ( 'NONE', *, *, #20637, .T. ) ;
#14599 = FACE_OUTER_BOUND ( 'NONE', #17859, .T. ) ;
#14600 = FACE_OUTER_BOUND ( 'NONE', #16132, .T. ) ;
#14601 = LINE ( 'NONE', #6939, #9076 ) ;
#14602 = AXIS2_PLACEMENT_3D ( 'NONE', #21448, #12279, #10073 ) ;
#14603 = EDGE_CURVE ( 'NONE', #4837, #12368, #13732, .T. ) ;
#14604 = LINE ( 'NONE', #19873, #7930 ) ;
#14605 = ORIENTED_EDGE ( 'NONE', *, *, #9460, .T. ) ;
#14606 = DIRECTION ( 'NONE',  ( 1.000000000000000000, 0.000000000000000000, 0.000000000000000000 ) ) ;
#14607 = ADVANCED_FACE ( 'NONE', ( #10660 ), #2752, .T. ) ;
#14608 = FILL_AREA_STYLE_COLOUR ( '', #18716 ) ;
#14609 = EDGE_LOOP ( 'NONE', ( #2769, #12035, #12520, #23154, #12362 ) ) ;
#14610 = ORIENTED_EDGE ( 'NONE', *, *, #12426, .T. ) ;
#14611 = CARTESIAN_POINT ( 'NONE',  ( -9.500000000000211386, 3.086737114211961064, 12.10674201446023091 ) ) ;
#14612 = CARTESIAN_POINT ( 'NONE',  ( -9.500000000000000000, -6.482511860946779655E-13, 6.206742014460234103 ) ) ;
#14613 = DIRECTION ( 'NONE',  ( 0.000000000000000000, 0.000000000000000000, -1.000000000000000000 ) ) ;
#14614 = EDGE_LOOP ( 'NONE', ( #15787, #13342, #8201, #21299, #7492 ) ) ;
#14615 = ORIENTED_EDGE ( 'NONE', *, *, #373, .T. ) ;
#14616 = VECTOR ( 'NONE', #17584, 1000.000000000000000 ) ;
#14617 = CARTESIAN_POINT ( 'NONE',  ( 0.000000000000000000, 0.000000000000000000, 38.00000000000003553 ) ) ;
#14618 = FACE_OUTER_BOUND ( 'NONE', #7753, .T. ) ;
#14619 = CARTESIAN_POINT ( 'NONE',  ( 0.000000000000000000, -45.00000000000000000, -8.673617379884035472E-16 ) ) ;
#14620 = CARTESIAN_POINT ( 'NONE',  ( 41.73082370883257397, -27.62204025492843940, -3.000000000000000000 ) ) ;
#14621 = LINE ( 'NONE', #15193, #9952 ) ;
#14622 = CONICAL_SURFACE ( 'NONE', #11484, 2.024999999999999911, 0.7853981633974743692 ) ;
#14623 = AXIS2_PLACEMENT_3D ( 'NONE', #23213, #11958, #13935 ) ;
#14624 = CIRCLE ( 'NONE', #12272, 5.000000000000007994 ) ;
#14625 = LINE ( 'NONE', #11060, #8687 ) ;
#14626 = CARTESIAN_POINT ( 'NONE',  ( 9.324366632326096311E-16, 9.000000000000000000, 77.99999999999998579 ) ) ;
#14627 = CARTESIAN_POINT ( 'NONE',  ( -30.44534269664590198, -40.40463133211081015, -27.00000000000000000 ) ) ;
#14628 = EDGE_CURVE ( 'NONE', #3956, #16460, #13871, .T. ) ;
#14629 = ORIENTED_EDGE ( 'NONE', *, *, #10912, .F. ) ;
#14630 = APPLICATION_CONTEXT ( 'automotive_design' ) ;
#14631 = ADVANCED_FACE ( 'NONE', ( #933 ), #8588, .F. ) ;
#14632 = ORIENTED_EDGE ( 'NONE', *, *, #3223, .F. ) ;
#14633 = AXIS2_PLACEMENT_3D ( 'NONE', #19501, #17532, #21337 ) ;
#14634 = DIRECTION ( 'NONE',  ( -1.000000000000000000, 0.000000000000000000, 0.000000000000000000 ) ) ;
#14635 = LINE ( 'NONE', #11065, #12595 ) ;
#14636 = DIRECTION ( 'NONE',  ( -1.000000000000000000, 1.224646799147351482E-16, 0.000000000000000000 ) ) ;
#14637 = CARTESIAN_POINT ( 'NONE',  ( 0.000000000000000000, -15.03999999999999737, 2.200000000000000178 ) ) ;
#14638 = CIRCLE ( 'NONE', #12699, 4.172000000000008590 ) ;
#14639 = CARTESIAN_POINT ( 'NONE',  ( 33.99999999999998579, -5.000000000000013323, 11.00000000000000000 ) ) ;
#14640 = VERTEX_POINT ( 'NONE', #16038 ) ;
#14641 = CIRCLE ( 'NONE', #17773, 1.999999999999994449 ) ;
#14642 = CARTESIAN_POINT ( 'NONE',  ( 89.17200000000002547, 0.000000000000000000, 5.000000000000000888 ) ) ;
#14643 = AXIS2_PLACEMENT_3D ( 'NONE', #17374, #8081, #22994 ) ;
#14644 = ORIENTED_EDGE ( 'NONE', *, *, #677, .T. ) ;
#14645 = CARTESIAN_POINT ( 'NONE',  ( 30.31394790604173295, 39.41330121100981643, 12.00000000000000000 ) ) ;
#14646 = ORIENTED_EDGE ( 'NONE', *, *, #5110, .F. ) ;
#14647 = FACE_OUTER_BOUND ( 'NONE', #4433, .T. ) ;
#14648 = EDGE_LOOP ( 'NONE', ( #20337, #5230, #19650, #16144, #3111 ) ) ;
#14649 = CARTESIAN_POINT ( 'NONE',  ( -41.49999999999999289, 27.79189783386526358, 27.00000000000000000 ) ) ;
#14650 = DIRECTION ( 'NONE',  ( -1.000000000000000000, -0.000000000000000000, -0.000000000000000000 ) ) ;
#14651 = CYLINDRICAL_SURFACE ( 'NONE', #14234, 8.000000000000003553 ) ;
#14652 = AXIS2_PLACEMENT_3D ( 'NONE', #11908, #8374, #15827 ) ;
#14653 = AXIS2_PLACEMENT_3D ( 'NONE', #23555, #3288, #3058 ) ;
#14654 = DIRECTION ( 'NONE',  ( -0.000000000000000000, -0.000000000000000000, -1.000000000000000000 ) ) ;
#14655 = FACE_OUTER_BOUND ( 'NONE', #22851, .T. ) ;
#14656 = AXIS2_PLACEMENT_3D ( 'NONE', #19909, #5035, #1843 ) ;
#14657 = CARTESIAN_POINT ( 'NONE',  ( 7.685661446561619314, 5.583959896779020049, -8.259589141758144848 ) ) ;
#14658 = VERTEX_POINT ( 'NONE', #3112 ) ;
#14659 = ORIENTED_EDGE ( 'NONE', *, *, #5440, .F. ) ;
#14660 = DIRECTION ( 'NONE',  ( -1.000000000000000000, 0.000000000000000000, 0.000000000000000000 ) ) ;
#14661 = EDGE_CURVE ( 'NONE', #19085, #5096, #9664, .T. ) ;
#14662 = ADVANCED_FACE ( 'NONE', ( #4845 ), #1425, .F. ) ;
#14663 = DIRECTION ( 'NONE',  ( 0.000000000000000000, -1.000000000000000000, 0.000000000000000000 ) ) ;
#14664 = SURFACE_SIDE_STYLE ('',( #20173 ) ) ;
#14665 = ORIENTED_EDGE ( 'NONE', *, *, #13985, .F. ) ;
#14666 = AXIS2_PLACEMENT_3D ( 'NONE', #17845, #4796, #19432 ) ;
#14667 = LINE ( 'NONE', #16725, #7883 ) ;
#14668 = CIRCLE ( 'NONE', #4168, 5.000000000000000888 ) ;
#14669 = DIRECTION ( 'NONE',  ( -0.000000000000000000, 0.000000000000000000, 1.000000000000000000 ) ) ;
#14670 = ORIENTED_EDGE ( 'NONE', *, *, #10438, .T. ) ;
#14671 = CARTESIAN_POINT ( 'NONE',  ( 0.3000000000000023204, 0.000000000000000000, 0.000000000000000000 ) ) ;
#14672 = DIRECTION ( 'NONE',  ( 0.000000000000000000, 0.000000000000000000, 1.000000000000000000 ) ) ;
#14673 = DIRECTION ( 'NONE',  ( 0.000000000000000000, 0.000000000000000000, 1.000000000000000000 ) ) ;
#14674 = CIRCLE ( 'NONE', #20872, 10.50249999999999950 ) ;
#14675 = DIRECTION ( 'NONE',  ( -0.000000000000000000, -0.000000000000000000, -1.000000000000000000 ) ) ;
#14676 =( BOUNDED_CURVE ( )  B_SPLINE_CURVE ( 2, ( #18078, #18202, #15991, #14163, #15881, #12553, #4921, #1243, #8657, #8904, #12441 ),
 .UNSPECIFIED., .F., .T. ) 
 B_SPLINE_CURVE_WITH_KNOTS ( ( 3, 2, 2, 2, 2, 3 ),
 ( 0.5000000000000000000, 0.5200000000000000178, 0.5400000000000000355, 0.5600000000000001643, 0.5800000000000000711, 0.6000000000000000888 ),
 .UNSPECIFIED. ) 
 CURVE ( )  GEOMETRIC_REPRESENTATION_ITEM ( )  RATIONAL_B_SPLINE_CURVE ( ( 1.000000000000000000, 0.9510565162951535312, 1.000000000000000000, 0.9510565162951535312, 1.000000000000000000, 0.9510565162951535312, 1.000000000000000000, 0.9510565162951535312, 1.000000000000000000, 0.9510565162951533091, 1.000000000000000222 ) ) 
 REPRESENTATION_ITEM ( '' )  );
#14677 = CARTESIAN_POINT ( 'NONE',  ( -7.022953521754877748, -5.102474405760673015, 3.833165578109188676 ) ) ;
#14678 = ORIENTED_EDGE ( 'NONE', *, *, #4345, .T. ) ;
#14679 = ORIENTED_EDGE ( 'NONE', *, *, #8800, .F. ) ;
#14680 = ORIENTED_EDGE ( 'NONE', *, *, #14661, .F. ) ;
#14681 = AXIS2_PLACEMENT_3D ( 'NONE', #22612, #7359, #17106 ) ;
#14682 = ADVANCED_FACE ( 'NONE', ( #10428 ), #22444, .F. ) ;
#14683 = ORIENTED_EDGE ( 'NONE', *, *, #1516, .T. ) ;
#14684 = ORIENTED_EDGE ( 'NONE', *, *, #13207, .F. ) ;
#14685 = FACE_BOUND ( 'NONE', #20848, .T. ) ;
#14686 = AXIS2_PLACEMENT_3D ( 'NONE', #1012, #23221, #8437 ) ;
#14687 = EDGE_CURVE ( 'NONE', #9227, #7988, #19843, .T. ) ;
#14688 = DIRECTION ( 'NONE',  ( -0.000000000000000000, -0.000000000000000000, -1.000000000000000000 ) ) ;
#14689 = ORIENTED_EDGE ( 'NONE', *, *, #2492, .T. ) ;
#14690 = ORIENTED_EDGE ( 'NONE', *, *, #21397, .T. ) ;
#14691 = EDGE_CURVE ( 'NONE', #12916, #17567, #15813, .T. ) ;
#14692 = ADVANCED_FACE ( 'NONE', ( #21313 ), #22840, .T. ) ;
#14693 = EDGE_CURVE ( 'NONE', #18733, #10181, #11506, .T. ) ;
#14694 = LINE ( 'NONE', #1290, #20830 ) ;
#14695 = VERTEX_POINT ( 'NONE', #6548 ) ;
#14696 = DIRECTION ( 'NONE',  ( 1.000000000000000000, 0.000000000000000000, 0.000000000000000000 ) ) ;
#14697 = DIRECTION ( 'NONE',  ( 0.000000000000000000, -1.000000000000000000, 0.000000000000000000 ) ) ;
#14698 = DIRECTION ( 'NONE',  ( -1.000000000000000000, 0.000000000000000000, -0.000000000000000000 ) ) ;
#14699 = DIRECTION ( 'NONE',  ( 0.000000000000000000, -1.000000000000000000, 0.000000000000000000 ) ) ;
#14700 = DIRECTION ( 'NONE',  ( 1.000000000000000000, 0.000000000000000000, 0.000000000000000000 ) ) ;
#14701 = DIRECTION ( 'NONE',  ( 1.000000000000000000, 2.775557561562888984E-15, 0.000000000000000000 ) ) ;
#14702 = DIRECTION ( 'NONE',  ( -1.000000000000000000, -1.224606353822377258E-16, -0.000000000000000000 ) ) ;
#14703 = EDGE_LOOP ( 'NONE', ( #1114, #17942, #15356, #1157, #8418, #228, #10703, #22747, #773, #12483, #5785, #7147, #13584, #14583, #22054, #12022, #16358, #10678, #11433, #12006, #381, #4704, #17491, #3715 ) ) ;
#14704 = CARTESIAN_POINT ( 'NONE',  ( -7.022953521754877748, -5.102474405760673015, 7.833165578109188232 ) ) ;
#14705 = ORIENTED_EDGE ( 'NONE', *, *, #10913, .T. ) ;
#14706 = SHAPE_DEFINITION_REPRESENTATION ( #3024, #9527 ) ;
#14707 = EDGE_CURVE ( 'NONE', #19489, #5826, #14641, .T. ) ;
#14708 = FACE_OUTER_BOUND ( 'NONE', #21439, .T. ) ;
#14709 = VERTEX_POINT ( 'NONE', #13982 ) ;
#14710 = VERTEX_POINT ( 'NONE', #4717 ) ;
#14711 = DIRECTION ( 'NONE',  ( -0.000000000000000000, -0.000000000000000000, 1.000000000000000000 ) ) ;
#14712 = CARTESIAN_POINT ( 'NONE',  ( -8.680847955710813579, -2.820578480814258437, -9.733165578109186811 ) ) ;
#14713 = CARTESIAN_POINT ( 'NONE',  ( -42.00000000000000000, -26.82133436441678853, 12.00000000000000000 ) ) ;
#14714 = CARTESIAN_POINT ( 'NONE',  ( 0.000000000000000000, 45.00000000000000000, -8.673617379884035472E-16 ) ) ;
#14715 = CARTESIAN_POINT ( 'NONE',  ( 35.99999999999999289, -51.00000000000000711, 0.5000000000000000000 ) ) ;
#14716 = ADVANCED_FACE ( 'NONE', ( #19598, #6905 ), #1062, .F. ) ;
#14717 = DIRECTION ( 'NONE',  ( 1.000000000000000000, 0.000000000000000000, 0.000000000000000000 ) ) ;
#14718 = EDGE_CURVE ( 'NONE', #23514, #14903, #7240, .T. ) ;
#14719 = CARTESIAN_POINT ( 'NONE',  ( 41.00000000000000000, 3.999999999999987121, 10.49999999999999822 ) ) ;
#14720 = ORIENTED_EDGE ( 'NONE', *, *, #12914, .F. ) ;
#14721 = CIRCLE ( 'NONE', #4213, 5.400000000000001243 ) ;
#14722 = CARTESIAN_POINT ( 'NONE',  ( 5.871322893124551356, -8.081182679343980269, -6.906742014460233392 ) ) ;
#14723 = ORIENTED_EDGE ( 'NONE', *, *, #13755, .F. ) ;
#14724 = FACE_OUTER_BOUND ( 'NONE', #5494, .T. ) ;
#14725 = DIRECTION ( 'NONE',  ( -1.000000000000000000, 0.000000000000000000, 0.000000000000000000 ) ) ;
#14726 = DIRECTION ( 'NONE',  ( 0.000000000000000000, 0.000000000000000000, 1.000000000000000000 ) ) ;
#14727 = CARTESIAN_POINT ( 'NONE',  ( 16.44572538483723534, 6.755397553796131049, 6.683320200552552492 ) ) ;
#14728 = CARTESIAN_POINT ( 'NONE',  ( 1.999999999999994449, 45.00000000000000000, -23.99999999999999645 ) ) ;
#14729 = DIRECTION ( 'NONE',  ( 0.8571673007021116675, 1.049727191138617833E-16, -0.5150380749100552658 ) ) ;
#14730 = CARTESIAN_POINT ( 'NONE',  ( 0.000000000000000000, 0.000000000000000000, 0.000000000000000000 ) ) ;
#14731 = ORIENTED_EDGE ( 'NONE', *, *, #3459, .F. ) ;
#14732 = ORIENTED_EDGE ( 'NONE', *, *, #3791, .T. ) ;
#14733 = CARTESIAN_POINT ( 'NONE',  ( 5.871322893123449127, 8.081182679344781405, 7.506742014460233037 ) ) ;
#14734 = VERTEX_POINT ( 'NONE', #21896 ) ;
#14735 = AXIS2_PLACEMENT_3D ( 'NONE', #439, #5809, #19108 ) ;
#14736 = VERTEX_POINT ( 'NONE', #5535 ) ;
#14737 = VECTOR ( 'NONE', #23599, 1000.000000000000000 ) ;
#14738 = CARTESIAN_POINT ( 'NONE',  ( 35.99999999999999289, 50.99999999999999289, 12.50000000000000000 ) ) ;
#14739 = DIRECTION ( 'NONE',  ( 0.000000000000000000, -1.000000000000000000, 0.000000000000000000 ) ) ;
#14740 = DIRECTION ( 'NONE',  ( 1.000000000000000000, -0.000000000000000000, 0.000000000000000000 ) ) ;
#14741 = FACE_OUTER_BOUND ( 'NONE', #17239, .T. ) ;
#14742 = CARTESIAN_POINT ( 'NONE',  ( 0.000000000000000000, 0.000000000000000000, 0.000000000000000000 ) ) ;
#14743 = CARTESIAN_POINT ( 'NONE',  ( 41.00000000000000000, -4.000000000000015099, 10.49999999999999822 ) ) ;
#14744 = VECTOR ( 'NONE', #10328, 1000.000000000000114 ) ;
#14745 = EDGE_CURVE ( 'NONE', #17802, #14826, #18242, .T. ) ;
#14746 = DIRECTION ( 'NONE',  ( 0.000000000000000000, 0.000000000000000000, 1.000000000000000000 ) ) ;
#14747 = ORIENTED_EDGE ( 'NONE', *, *, #3941, .F. ) ;
#14748 = CARTESIAN_POINT ( 'NONE',  ( -33.24999999999999289, 29.50000000000000000, 14.00000000000000178 ) ) ;
#14749 = CARTESIAN_POINT ( 'NONE',  ( 2.000000000000000000, 2.449293598294706414E-16, 0.4999999999999995559 ) ) ;
#14750 = DIRECTION ( 'NONE',  ( 1.000000000000000000, 0.000000000000000000, 0.000000000000000000 ) ) ;
#14751 = CARTESIAN_POINT ( 'NONE',  ( -34.10000000000000142, 29.50000000000000000, 27.00000000000000000 ) ) ;
#14752 = DIRECTION ( 'NONE',  ( 0.000000000000000000, 0.000000000000000000, -1.000000000000000000 ) ) ;
#14753 = CARTESIAN_POINT ( 'NONE',  ( -8.680847955711200825, 2.820578480813073607, -9.533165578109187521 ) ) ;
#14754 = DIRECTION ( 'NONE',  ( -0.5735764363510519326, 0.8191520442889876907, 1.003171929053519816E-16 ) ) ;
#14755 = EDGE_LOOP ( 'NONE', ( #19109, #11693, #2079, #20748 ) ) ;
#14756 = FACE_OUTER_BOUND ( 'NONE', #6017, .T. ) ;
#14757 = ORIENTED_EDGE ( 'NONE', *, *, #22099, .F. ) ;
#14758 = FACE_OUTER_BOUND ( 'NONE', #13310, .T. ) ;
#14759 = AXIS2_PLACEMENT_3D ( 'NONE', #5997, #157, #13435 ) ;
#14760 = EDGE_CURVE ( 'NONE', #9485, #758, #12288, .T. ) ;
#14761 = VERTEX_POINT ( 'NONE', #18479 ) ;
#14762 = SHAPE_REPRESENTATION_RELATIONSHIP ( 'NONE' , 'NONE' ,  #2057, #18057 ) ;
#14763 = DIRECTION ( 'NONE',  ( 0.000000000000000000, -1.000000000000000000, 0.000000000000000000 ) ) ;
#14764 = CARTESIAN_POINT ( 'NONE',  ( -5.871322893124554021, 8.081182679343978492, -2.759589141758142627 ) ) ;
#14765 = ADVANCED_FACE ( 'NONE', ( #5181 ), #8946, .T. ) ;
#14766 = CARTESIAN_POINT ( 'NONE',  ( 3.890962118697714531E-15, 15.50000000000000000, 19.70000000000000284 ) ) ;
#14767 = ADVANCED_FACE ( 'NONE', ( #16644 ), #20502, .F. ) ;
#14768 = DIRECTION ( 'NONE',  ( 0.000000000000000000, 0.4999999999999989453, -0.8660254037844392627 ) ) ;
#14769 = EDGE_CURVE ( 'NONE', #2336, #20664, #23843, .T. ) ;
#14770 = CARTESIAN_POINT ( 'NONE',  ( -6.822232771736903637E-13, 9.988891130263535700, -4.559589141758142894 ) ) ;
#14771 = VERTEX_POINT ( 'NONE', #12053 ) ;
#14772 = DIRECTION ( 'NONE',  ( 0.000000000000000000, -1.000000000000000000, 0.000000000000000000 ) ) ;
#14773 = CARTESIAN_POINT ( 'NONE',  ( 34.10000000000000142, -29.50000000000000355, 11.50000000000000000 ) ) ;
#14774 = ORIENTED_EDGE ( 'NONE', *, *, #20450, .F. ) ;
#14775 = FACE_OUTER_BOUND ( 'NONE', #11712, .T. ) ;
#14776 = AXIS2_PLACEMENT_3D ( 'NONE', #5184, #22035, #12491 ) ;
#14777 = EDGE_LOOP ( 'NONE', ( #9114, #6935, #10026, #22313, #5171 ) ) ;
#14778 = CARTESIAN_POINT ( 'NONE',  ( 30.31394790604173295, 39.41330121100981643, 11.00000000000000000 ) ) ;
#14779 = CARTESIAN_POINT ( 'NONE',  ( 14.67187117805616303, -3.178673068337433349, 8.975236025575910048 ) ) ;
#14780 = CARTESIAN_POINT ( 'NONE',  ( 0.000000000000000000, 0.000000000000000000, 27.00000000000000000 ) ) ;
#14781 = ORIENTED_EDGE ( 'NONE', *, *, #1978, .T. ) ;
#14782 = DIRECTION ( 'NONE',  ( 0.000000000000000000, -1.000000000000000000, 0.000000000000000000 ) ) ;
#14783 = CARTESIAN_POINT ( 'NONE',  ( 7.937578510445358226, -3.514536757623690999, 12.49999999999999112 ) ) ;
#14784 = CARTESIAN_POINT ( 'NONE',  ( -2.935661446562617183, 9.035036904803758873, -3.806742014460233303 ) ) ;
#14785 = VERTEX_POINT ( 'NONE', #8529 ) ;
#14786 = ADVANCED_FACE ( 'NONE', ( #15974 ), #16219, .F. ) ;
#14787 = ORIENTED_EDGE ( 'NONE', *, *, #17966, .T. ) ;
#14788 = EDGE_CURVE ( 'NONE', #12663, #17474, #17688, .T. ) ;
#14789 = EDGE_LOOP ( 'NONE', ( #18174, #12584 ) ) ;
#14790 = AXIS2_PLACEMENT_3D ( 'NONE', #21200, #20962, #2899 ) ;
#14791 = VECTOR ( 'NONE', #21489, 1000.000000000000000 ) ;
#14792 = ORIENTED_EDGE ( 'NONE', *, *, #9705, .T. ) ;
#14793 = DIRECTION ( 'NONE',  ( 0.000000000000000000, 1.000000000000000000, 0.000000000000000000 ) ) ;
#14794 = CARTESIAN_POINT ( 'NONE',  ( -36.00000000000001421, 50.99999999999999289, 12.50000000000000000 ) ) ;
#14795 = EDGE_LOOP ( 'NONE', ( #7787, #14082, #7396, #3581 ) ) ;
#14796 = DIRECTION ( 'NONE',  ( -1.000000000000000000, 0.000000000000000000, 0.000000000000000000 ) ) ;
#14797 = ORIENTED_EDGE ( 'NONE', *, *, #20724, .F. ) ;
#14798 = LINE ( 'NONE', #8947, #10435 ) ;
#14799 = LINE ( 'NONE', #18356, #5899 ) ;
#14800 = DIRECTION ( 'NONE',  ( 0.000000000000000000, -1.000000000000000000, 0.000000000000000000 ) ) ;
#14801 = EDGE_CURVE ( 'NONE', #23778, #2165, #21678, .T. ) ;
#14802 = CARTESIAN_POINT ( 'NONE',  ( 35.99999999999999289, 50.99999999999999289, 0.000000000000000000 ) ) ;
#14803 = AXIS2_PLACEMENT_3D ( 'NONE', #11329, #2223, #20403 ) ;
#14804 = DIRECTION ( 'NONE',  ( -1.000000000000000000, -0.000000000000000000, -0.000000000000000000 ) ) ;
#14805 = CARTESIAN_POINT ( 'NONE',  ( 1.224646799147352468E-16, -12.99147757894464306, 8.749999999999998224 ) ) ;
#14806 = LINE ( 'NONE', #12625, #21680 ) ;
#14807 = ORIENTED_EDGE ( 'NONE', *, *, #14449, .F. ) ;
#14808 = CARTESIAN_POINT ( 'NONE',  ( 2.024999999999999911, -45.00000000000000000, 0.000000000000000000 ) ) ;
#14809 = ORIENTED_EDGE ( 'NONE', *, *, #4635, .T. ) ;
#14810 = EDGE_CURVE ( 'NONE', #20027, #4529, #4650, .T. ) ;
#14811 = EDGE_CURVE ( 'NONE', #11720, #22066, #633, .T. ) ;
#14812 = EDGE_LOOP ( 'NONE', ( #14358, #6033, #6226, #23580 ) ) ;
#14813 = EDGE_LOOP ( 'NONE', ( #12067, #15858, #21640, #10642 ) ) ;
#14814 = LINE ( 'NONE', #20219, #21642 ) ;
#14815 = CARTESIAN_POINT ( 'NONE',  ( -7.022953521754877748, -5.102474405760673015, -7.833165578109188232 ) ) ;
#14816 = COLOUR_RGB ( '',0.7921568627450980005, 0.8196078431372548767, 0.9333333333333333481 ) ;
#14817 = ORIENTED_EDGE ( 'NONE', *, *, #4120, .F. ) ;
#14818 = CARTESIAN_POINT ( 'NONE',  ( 71.09090909090909349, 4.172000000000015696, 5.109226446042767468E-16 ) ) ;
#14819 = CARTESIAN_POINT ( 'NONE',  ( -41.99999999999999289, 25.93535998569253920, -27.00000000000000000 ) ) ;
#14820 = DIRECTION ( 'NONE',  ( -0.7052211081716905916, 0.7089874389501501506, 0.000000000000000000 ) ) ;
#14821 = B_SPLINE_CURVE_WITH_KNOTS ( 'NONE', 3,
 ( #12000, #21544, #13862, #17621, #803, #6544, #6901, #4842, #17762, #15664, #1174, #19472, #12374, #8714, #8584, #23136, #6419, #16030, #13979, #4712, #21421, #21309, #4599, #17994, #23497, #2748, #6776, #14202, #19839, #10164, #16163, #928, #8352, #1529, #8942, #1764 ),
 .UNSPECIFIED., .F., .F.,
 ( 4, 2, 2, 2, 2, 2, 2, 2, 2, 2, 2, 2, 2, 2, 2, 2, 2, 4 ),
 ( 0.000000000000000000, 0.002901772246161908077, 0.003627215307702382711, 0.004352658369242857345, 0.005803544492323810949, 0.006528987553864288619, 0.007254430615404765421, 0.008705316738485725098, 0.01015620286156668217, 0.01160708898464764272, 0.01305797510772860326, 0.01450886123080956033, 0.01595974735389052088, 0.01741063347697148142, 0.01886151960005243849, 0.02031240572313339557, 0.02176329184621435611, 0.02321417796929531666 ),
 .UNSPECIFIED. ) ;
#14822 = DIRECTION ( 'NONE',  ( 0.000000000000000000, -1.000000000000000000, 0.000000000000000000 ) ) ;
#14823 = ORIENTED_EDGE ( 'NONE', *, *, #16679, .F. ) ;
#14824 = CARTESIAN_POINT ( 'NONE',  ( -34.10000000000000142, -29.49999999999999645, 11.50000000000000000 ) ) ;
#14825 = ORIENTED_EDGE ( 'NONE', *, *, #14188, .T. ) ;
#14826 = VERTEX_POINT ( 'NONE', #16091 ) ;
#14827 = FACE_OUTER_BOUND ( 'NONE', #7456, .T. ) ;
#14828 = DIRECTION ( 'NONE',  ( 0.7071067811865487940, 0.000000000000000000, 0.7071067811865463515 ) ) ;
#14829 = CARTESIAN_POINT ( 'NONE',  ( 1.041919733032276918, 45.00000000000000000, 0.000000000000000000 ) ) ;
#14830 = DIRECTION ( 'NONE',  ( -1.000000000000000000, 0.000000000000000000, 0.000000000000000000 ) ) ;
#14831 = EDGE_CURVE ( 'NONE', #18239, #3246, #19522, .T. ) ;
#14832 = DIRECTION ( 'NONE',  ( 0.000000000000000000, 0.000000000000000000, -1.000000000000000000 ) ) ;
#14833 = DIRECTION ( 'NONE',  ( 0.000000000000000000, 0.000000000000000000, -1.000000000000000000 ) ) ;
#14834 = EDGE_LOOP ( 'NONE', ( #24020, #10004, #11365, #7951 ) ) ;
#14835 = VERTEX_POINT ( 'NONE', #14266 ) ;
#14836 = AXIS2_PLACEMENT_3D ( 'NONE', #22015, #12723, #3462 ) ;
#14837 = CARTESIAN_POINT ( 'NONE',  ( -5.871322893123450015, -8.081182679344781405, 10.50674201446023304 ) ) ;
#14838 = EDGE_CURVE ( 'NONE', #3765, #3962, #5015, .T. ) ;
#14839 = VERTEX_POINT ( 'NONE', #10715 ) ;
#14840 = EDGE_CURVE ( 'NONE', #13274, #20276, #9955, .T. ) ;
#14841 = AXIS2_PLACEMENT_3D ( 'NONE', #12649, #220, #7498 ) ;
#14842 = EDGE_LOOP ( 'NONE', ( #11820, #23735, #8449, #15514, #22401, #13861 ) ) ;
#14843 = CARTESIAN_POINT ( 'NONE',  ( -31.74999999999995737, 6.123233995736767268E-16, -5.000000000000000888 ) ) ;
#14844 = ORIENTED_EDGE ( 'NONE', *, *, #13949, .T. ) ;
#14845 = CARTESIAN_POINT ( 'NONE',  ( 0.000000000000000000, 0.000000000000000000, 15.50000000000000000 ) ) ;
#14846 = CARTESIAN_POINT ( 'NONE',  ( 0.000000000000000000, 17.02535186363812514, -5.445458559198937287 ) ) ;
#14847 = DIRECTION ( 'NONE',  ( -1.000000000000000000, 0.000000000000000000, 0.000000000000000000 ) ) ;
#14848 = DIRECTION ( 'NONE',  ( -1.000000000000000000, -1.224606353822377258E-16, -0.000000000000000000 ) ) ;
#14849 = DIRECTION ( 'NONE',  ( 0.000000000000000000, 0.000000000000000000, 1.000000000000000000 ) ) ;
#14850 = AXIS2_PLACEMENT_3D ( 'NONE', #13031, #9351, #4264 ) ;
#14851 = AXIS2_PLACEMENT_3D ( 'NONE', #11635, #438, #6281 ) ;
#14852 = CARTESIAN_POINT ( 'NONE',  ( 0.000000000000000000, 0.000000000000000000, -12.50000000000000000 ) ) ;
#14853 = FACE_OUTER_BOUND ( 'NONE', #243, .T. ) ;
#14854 = CARTESIAN_POINT ( 'NONE',  ( 28.73477696352899358, -42.73830357953205805, 0.000000000000000000 ) ) ;
#14855 = AXIS2_PLACEMENT_3D ( 'NONE', #12619, #10890, #3716 ) ;
#14856 = CARTESIAN_POINT ( 'NONE',  ( 0.000000000000000000, -45.00000000000000000, -27.00000000000000000 ) ) ;
#14857 = CARTESIAN_POINT ( 'NONE',  ( 79.81818181818181301, 7.491529369508391930E-15, 0.000000000000000000 ) ) ;
#14858 = ORIENTED_EDGE ( 'NONE', *, *, #2942, .F. ) ;
#14859 = DIRECTION ( 'NONE',  ( -1.000000000000000000, -0.000000000000000000, -0.000000000000000000 ) ) ;
#14860 = ORIENTED_EDGE ( 'NONE', *, *, #19273, .T. ) ;
#14861 = DIRECTION ( 'NONE',  ( -0.000000000000000000, -0.000000000000000000, -1.000000000000000000 ) ) ;
#14862 = EDGE_CURVE ( 'NONE', #9263, #13492, #18603, .T. ) ;
#14863 = VERTEX_POINT ( 'NONE', #19658 ) ;
#14864 =( NAMED_UNIT ( * ) SI_UNIT ( $, .STERADIAN. ) SOLID_ANGLE_UNIT ( ) );
#14865 = ADVANCED_FACE ( 'NONE', ( #2932 ), #10360, .F. ) ;
#14866 = DIRECTION ( 'NONE',  ( -1.000000000000000000, 0.000000000000000000, 0.000000000000000000 ) ) ;
#14867 = VECTOR ( 'NONE', #15334, 1000.000000000000000 ) ;
#14868 = CIRCLE ( 'NONE', #23470, 1.999999999999994449 ) ;
#14869 = AXIS2_PLACEMENT_3D ( 'NONE', #4636, #12037, #19508 ) ;
#14870 = FACE_OUTER_BOUND ( 'NONE', #20442, .T. ) ;
#14871 = AXIS2_PLACEMENT_3D ( 'NONE', #10280, #23473, #4819 ) ;
#14872 = AXIS2_PLACEMENT_3D ( 'NONE', #668, #17481, #782 ) ;
#14873 = AXIS2_PLACEMENT_3D ( 'NONE', #16846, #12831, #4057 ) ;
#14874 = CARTESIAN_POINT ( 'NONE',  ( -1.999999999999994449, -45.00000000000000000, -27.00000000000000000 ) ) ;
#14875 = CARTESIAN_POINT ( 'NONE',  ( -2.935661446561384391, -9.035036904804158553, -9.459589141758144137 ) ) ;
#14876 = VERTEX_POINT ( 'NONE', #1698 ) ;
#14877 = VERTEX_POINT ( 'NONE', #12898 ) ;
#14878 = CARTESIAN_POINT ( 'NONE',  ( -41.99999999999997158, -25.22443390181683043, -1.500000000000000000 ) ) ;
#14879 = DIRECTION ( 'NONE',  ( 0.000000000000000000, 0.000000000000000000, 1.000000000000000000 ) ) ;
#14880 = EDGE_CURVE ( 'NONE', #22249, #23011, #19346, .T. ) ;
#14881 = ORIENTED_EDGE ( 'NONE', *, *, #8215, .T. ) ;
#14882 = DIRECTION ( 'NONE',  ( 1.000000000000000000, 0.000000000000000000, 0.000000000000000000 ) ) ;
#14883 = VECTOR ( 'NONE', #3498, 1000.000000000000000 ) ;
#14884 = ADVANCED_FACE ( 'NONE', ( #20602 ), #10697, .T. ) ;
#14885 = AXIS2_PLACEMENT_3D ( 'NONE', #9890, #7807, #168 ) ;
#14886 = ORIENTED_EDGE ( 'NONE', *, *, #5335, .F. ) ;
#14887 = AXIS2_PLACEMENT_3D ( 'NONE', #13149, #20612, #18418 ) ;
#14888 = DIRECTION ( 'NONE',  ( -1.000000000000000000, -0.000000000000000000, -0.000000000000000000 ) ) ;
#14889 = AXIS2_PLACEMENT_3D ( 'NONE', #18656, #5366, #16797 ) ;
#14890 = DIRECTION ( 'NONE',  ( 0.000000000000000000, 0.000000000000000000, 1.000000000000000000 ) ) ;
#14891 = VECTOR ( 'NONE', #18282, 1000.000000000000000 ) ;
#14892 = DIRECTION ( 'NONE',  ( 0.000000000000000000, 0.000000000000000000, -1.000000000000000000 ) ) ;
#14893 = ORIENTED_EDGE ( 'NONE', *, *, #10177, .F. ) ;
#14894 = AXIS2_PLACEMENT_3D ( 'NONE', #1623, #9386, #14672 ) ;
#14895 = LINE ( 'NONE', #3691, #12473 ) ;
#14896 = ADVANCED_FACE ( 'NONE', ( #1927 ), #5362, .T. ) ;
#14897 = DIRECTION ( 'NONE',  ( -1.000000000000000000, 0.000000000000000000, 0.000000000000000000 ) ) ;
#14898 = DIRECTION ( 'NONE',  ( 0.7052211081716905916, 0.7089874389501501506, 0.000000000000000000 ) ) ;
#14899 = CIRCLE ( 'NONE', #21146, 5.000000000000007994 ) ;
#14900 = CARTESIAN_POINT ( 'NONE',  ( -34.00000000000000000, 4.999999999999999112, 9.500000000000000000 ) ) ;
#14901 = CARTESIAN_POINT ( 'NONE',  ( -8.680847955711007202, -5.923547351154968927E-13, 3.633165578109188054 ) ) ;
#14902 = ORIENTED_EDGE ( 'NONE', *, *, #14100, .F. ) ;
#14903 = VERTEX_POINT ( 'NONE', #22200 ) ;
#14904 = CIRCLE ( 'NONE', #915, 1.999999999999994449 ) ;
#14906 = AXIS2_PLACEMENT_3D ( 'NONE', #19296, #12194, #1121 ) ;
#14905 = CARTESIAN_POINT ( 'NONE',  ( 68.76159002345582394, 5.000000000000015987, 0.000000000000000000 ) ) ;
#14907 = AXIS2_PLACEMENT_3D ( 'NONE', #3002, #12251, #6900 ) ;
#14908 = CYLINDRICAL_SURFACE ( 'NONE', #23124, 1.000000000000000888 ) ;
#14909 = VERTEX_POINT ( 'NONE', #14963 ) ;
#14910 = ADVANCED_FACE ( 'NONE', ( #14485, #9244 ), #11175, .T. ) ;
#14911 = CARTESIAN_POINT ( 'NONE',  ( 76.03431729618309021, 5.000000000000015987, 0.000000000000000000 ) ) ;
#14912 = CIRCLE ( 'NONE', #2868, 49.99999999999998579 ) ;
#14913 = ORIENTED_EDGE ( 'NONE', *, *, #17891, .F. ) ;
#14914 = DIRECTION ( 'NONE',  ( -0.000000000000000000, -0.000000000000000000, -1.000000000000000000 ) ) ;
#14915 = ADVANCED_FACE ( 'NONE', ( #20482 ), #18652, .F. ) ;
#14916 = DIRECTION ( 'NONE',  ( 0.000000000000000000, -1.000000000000000000, 0.000000000000000000 ) ) ;
#14917 = LINE ( 'NONE', #13099, #1713 ) ;
#14918 = DIRECTION ( 'NONE',  ( -1.000000000000000000, 0.000000000000000000, 0.000000000000000000 ) ) ;
#14919 = TOROIDAL_SURFACE ( 'NONE', #3257, 2.000000000000000000, 1.000000000000000000 ) ;
#14920 = DIRECTION ( 'NONE',  ( -1.000000000000000000, 0.000000000000000000, 0.000000000000000000 ) ) ;
#14921 = CARTESIAN_POINT ( 'NONE',  ( 42.00000000000000000, -4.000000000000015099, 10.49999999999999822 ) ) ;
#14922 = CARTESIAN_POINT ( 'NONE',  ( 81.27272727272728048, 7.491529369508391930E-15, 0.000000000000000000 ) ) ;
#14923 = EDGE_LOOP ( 'NONE', ( #1081, #16518, #19382, #22465 ) ) ;
#14924 = VECTOR ( 'NONE', #17237, 1000.000000000000000 ) ;
#14925 = ORIENTED_EDGE ( 'NONE', *, *, #10940, .F. ) ;
#14926 = CARTESIAN_POINT ( 'NONE',  ( -2.682529543899159208, -8.255977015246598327, 4.033165578109189298 ) ) ;
#14927 = VERTEX_POINT ( 'NONE', #15567 ) ;
#14928 = CIRCLE ( 'NONE', #12206, 4.000000000000000000 ) ;
#14929 = AXIS2_PLACEMENT_3D ( 'NONE', #15045, #22515, #18842 ) ;
#14930 = VECTOR ( 'NONE', #9219, 1000.000000000000000 ) ;
#14931 = APPLICATION_PROTOCOL_DEFINITION ( 'draft international standard', 'automotive_design', 1998, #13864 ) ;
#14932 = ORIENTED_EDGE ( 'NONE', *, *, #2348, .F. ) ;
#14933 = ORIENTED_EDGE ( 'NONE', *, *, #346, .F. ) ;
#14934 = CARTESIAN_POINT ( 'NONE',  ( 41.99999999999997158, -25.22443390181681622, -3.000000000000000000 ) ) ;
#14935 = CARTESIAN_POINT ( 'NONE',  ( -9.499999999999790390, -3.086737114213257804, -3.159589141758143871 ) ) ;
#14936 = DIRECTION ( 'NONE',  ( 0.000000000000000000, 1.000000000000000000, -9.256405414277000802E-16 ) ) ;
#14937 = ORIENTED_EDGE ( 'NONE', *, *, #16385, .F. ) ;
#14938 = DIRECTION ( 'NONE',  ( 0.000000000000000000, -1.000000000000000000, 0.000000000000000000 ) ) ;
#14939 = LINE ( 'NONE', #16895, #16977 ) ;
#14940 = CARTESIAN_POINT ( 'NONE',  ( 0.000000000000000000, -13.66196005206961850, -3.918670437617226110 ) ) ;
#14941 = CIRCLE ( 'NONE', #11824, 14.72592346043842326 ) ;
#14942 = CARTESIAN_POINT ( 'NONE',  ( 0.000000000000000000, -13.61176534793449200, 10.13961790095610560 ) ) ;
#14943 = ORIENTED_EDGE ( 'NONE', *, *, #23900, .T. ) ;
#14944 = DIRECTION ( 'NONE',  ( 0.000000000000000000, -1.000000000000000000, 0.000000000000000000 ) ) ;
#14945 = VERTEX_POINT ( 'NONE', #21202 ) ;
#14946 = VECTOR ( 'NONE', #12339, 1000.000000000000000 ) ;
#14947 = EDGE_CURVE ( 'NONE', #12918, #18883, #7870, .T. ) ;
#14948 = CIRCLE ( 'NONE', #19262, 1.000000000000000888 ) ;
#14949 = ADVANCED_FACE ( 'NONE', ( #11655 ), #3994, .F. ) ;
#14950 = ORIENTED_EDGE ( 'NONE', *, *, #24057, .F. ) ;
#14951 = CARTESIAN_POINT ( 'NONE',  ( -7.685661446561619314, -5.583959896779019161, -7.259589141758143960 ) ) ;
#14952 = CARTESIAN_POINT ( 'NONE',  ( 29.00000000000000711, -29.50000000000000711, 27.00000000000000000 ) ) ;
#14953 = CIRCLE ( 'NONE', #3684, 10.49999999999999822 ) ;
#14954 = CARTESIAN_POINT ( 'NONE',  ( 5.000000000000000000, -2.342598717236905603, 4.057500000000010765 ) ) ;
#14955 = CARTESIAN_POINT ( 'NONE',  ( 7.564539288232062120, -4.357045548396844659, -12.46583266205519713 ) ) ;
#14956 =( NAMED_UNIT ( * ) PLANE_ANGLE_UNIT ( ) SI_UNIT ( $, .RADIAN. ) );
#14957 = ORIENTED_EDGE ( 'NONE', *, *, #1321, .T. ) ;
#14958 = ORIENTED_EDGE ( 'NONE', *, *, #11707, .F. ) ;
#14959 = ORIENTED_EDGE ( 'NONE', *, *, #23643, .F. ) ;
#14960 = ORIENTED_EDGE ( 'NONE', *, *, #10492, .T. ) ;
#14961 = SHAPE_REPRESENTATION_RELATIONSHIP ( 'NONE' , 'NONE' ,  #23456, #20093 ) ;
#14962 = CIRCLE ( 'NONE', #6028, 1.000000000000000444 ) ;
#14963 = CARTESIAN_POINT ( 'NONE',  ( -40.00000000000000000, 29.49999999999999645, 11.00000000000000000 ) ) ;
#14964 = DIRECTION ( 'NONE',  ( -1.000000000000000000, -0.000000000000000000, -0.000000000000000000 ) ) ;
#14965 = CIRCLE ( 'NONE', #12265, 4.172000000000008590 ) ;
#14966 = ADVANCED_FACE ( 'NONE', ( #11413 ), #17339, .F. ) ;
#14967 = AXIS2_PLACEMENT_3D ( 'NONE', #4601, #4227, #4346 ) ;
#14968 = CARTESIAN_POINT ( 'NONE',  ( -18.50000000000000000, 0.000000000000000000, 15.50000000000000000 ) ) ;
#14969 = CARTESIAN_POINT ( 'NONE',  ( 4.489900896931573904, 1.117316575569334134E-15, 8.500000000000000000 ) ) ;
#14970 = CARTESIAN_POINT ( 'NONE',  ( 0.000000000000000000, 0.000000000000000000, 15.00000000000000178 ) ) ;
#14971 = ADVANCED_FACE ( 'NONE', ( #2404 ), #22662, .F. ) ;
#14972 = CIRCLE ( 'NONE', #11859, 1.500000000000000222 ) ;
#14973 = CYLINDRICAL_SURFACE ( 'NONE', #16442, 5.100000000000000533 ) ;
#14974 = EDGE_LOOP ( 'NONE', ( #15403, #10692, #23597, #7272, #16776 ) ) ;
#14975 = ADVANCED_FACE ( 'NONE', ( #22795 ), #17286, .T. ) ;
#14976 = CARTESIAN_POINT ( 'NONE',  ( 86.21613547800127719, 7.562528597612068045E-15, 0.000000000000000000 ) ) ;
#14977 = EDGE_CURVE ( 'NONE', #21663, #18617, #4367, .T. ) ;
#14978 = CARTESIAN_POINT ( 'NONE',  ( -41.00000000000000000, 26.23076770084981391, 12.00000000000000000 ) ) ;
#14979 = DIRECTION ( 'NONE',  ( -1.000000000000000000, 4.613626265895763066E-16, 0.000000000000000000 ) ) ;
#14980 = ADVANCED_FACE ( 'NONE', ( #6682 ), #3133, .F. ) ;
#14981 = DIRECTION ( 'NONE',  ( -1.000000000000000000, 0.000000000000000000, 0.000000000000000000 ) ) ;
#14982 = AXIS2_PLACEMENT_3D ( 'NONE', #17738, #13838, #6525 ) ;
#14983 = DIRECTION ( 'NONE',  ( 0.5735764363510424957, 0.8191520442889943521, 0.000000000000000000 ) ) ;
#14984 = VERTEX_POINT ( 'NONE', #13891 ) ;
#14985 = AXIS2_PLACEMENT_3D ( 'NONE', #16526, #18484, #16289 ) ;
#14986 = ORIENTED_EDGE ( 'NONE', *, *, #17849, .T. ) ;
#14987 = CARTESIAN_POINT ( 'NONE',  ( -23.89999999999999858, -29.50000000000001066, -27.00000000000000000 ) ) ;
#14988 = VECTOR ( 'NONE', #17848, 1000.000000000000000 ) ;
#14989 = VERTEX_POINT ( 'NONE', #10192 ) ;
#14990 = CARTESIAN_POINT ( 'NONE',  ( 5.871322893124551356, -8.081182679343980269, -9.759589141758143072 ) ) ;
#14991 = VERTEX_POINT ( 'NONE', #16192 ) ;
#14992 = FACE_BOUND ( 'NONE', #7202, .T. ) ;
#14993 = DIRECTION ( 'NONE',  ( 0.000000000000000000, -1.000000000000000000, 0.000000000000000000 ) ) ;
#14994 = DIRECTION ( 'NONE',  ( 1.000000000000000000, 0.000000000000000000, 0.000000000000000000 ) ) ;
#14995 = DIRECTION ( 'NONE',  ( 0.000000000000000000, -1.000000000000000000, 0.000000000000000000 ) ) ;
#14996 = LINE ( 'NONE', #9731, #15811 ) ;
#14997 = EDGE_CURVE ( 'NONE', #17352, #105, #5267, .T. ) ;
#14998 = CARTESIAN_POINT ( 'NONE',  ( 7.685661446562381371, -5.583959896777971110, -7.859589141758143604 ) ) ;
#14999 = ORIENTED_EDGE ( 'NONE', *, *, #19550, .F. ) ;
#15000 = AXIS2_PLACEMENT_3D ( 'NONE', #17071, #16714, #17187 ) ;
#15001 = DIRECTION ( 'NONE',  ( 1.000000000000000000, 2.600433232233976523E-16, 0.000000000000000000 ) ) ;
#15002 = CARTESIAN_POINT ( 'NONE',  ( -7.561939491010504000, 5.750397476200735269, 11.99999999999999822 ) ) ;
#15004 = ADVANCED_FACE ( 'NONE', ( #21333 ), #6837, .T. ) ;
#15003 = CONICAL_SURFACE ( 'NONE', #18931, 5.000000000000007994, 0.9599310885968855844 ) ;
#15005 = ORIENTED_EDGE ( 'NONE', *, *, #17422, .F. ) ;
#15006 = DIRECTION ( 'NONE',  ( -1.000000000000000000, -0.000000000000000000, -0.000000000000000000 ) ) ;
#15007 = CARTESIAN_POINT ( 'NONE',  ( 23.84999999999999432, -15.03999999999999559, -27.00000000000000000 ) ) ;
#15008 = AXIS2_PLACEMENT_3D ( 'NONE', #19580, #1273, #10288 ) ;
#15009 = CYLINDRICAL_SURFACE ( 'NONE', #3466, 5.000000000000000888 ) ;
#15010 = CARTESIAN_POINT ( 'NONE',  ( 23.00000000000000000, 12.00453763395397466, 7.608955687739546114 ) ) ;
#15011 = CARTESIAN_POINT ( 'NONE',  ( 7.000000000000000888, 0.000000000000000000, 0.000000000000000000 ) ) ;
#15012 = CYLINDRICAL_SURFACE ( 'NONE', #9452, 9.500000000000000000 ) ;
#15013 = ORIENTED_EDGE ( 'NONE', *, *, #8968, .T. ) ;
#15014 = FACE_OUTER_BOUND ( 'NONE', #23111, .T. ) ;
#15015 = DIRECTION ( 'NONE',  ( 0.000000000000000000, -0.000000000000000000, -1.000000000000000000 ) ) ;
#15016 = CARTESIAN_POINT ( 'NONE',  ( 66.72727272727273373, -4.172000000000000597, 5.616230220889771312E-16 ) ) ;
#15017 = CARTESIAN_POINT ( 'NONE',  ( 10.49999999999999822, 0.000000000000000000, -2.499999999999999556 ) ) ;
#15018 = CIRCLE ( 'NONE', #11519, 5.000000000000007994 ) ;
#15019 = DIRECTION ( 'NONE',  ( -1.000000000000000000, 0.000000000000000000, 0.000000000000000000 ) ) ;
#15020 = ORIENTED_EDGE ( 'NONE', *, *, #19171, .F. ) ;
#15021 = PRODUCT_DEFINITION_SHAPE ( 'NONE', 'NONE',  #16174 ) ;
#15022 = ORIENTED_EDGE ( 'NONE', *, *, #5572, .T. ) ;
#15023 = VECTOR ( 'NONE', #372, 1000.000000000000000 ) ;
#15024 = AXIS2_PLACEMENT_3D ( 'NONE', #15976, #23436, #17940 ) ;
#15025 = ORIENTED_EDGE ( 'NONE', *, *, #12498, .T. ) ;
#15026 = EDGE_CURVE ( 'NONE', #5560, #15166, #8368, .T. ) ;
#15027 = ORIENTED_EDGE ( 'NONE', *, *, #20655, .T. ) ;
#15028 = CARTESIAN_POINT ( 'NONE',  ( 0.000000000000000000, -9.239931321968246181, 10.79948145182496511 ) ) ;
#15029 = CARTESIAN_POINT ( 'NONE',  ( -40.00000000000000000, -29.49999999999999645, 12.00000000000000000 ) ) ;
#15030 = CARTESIAN_POINT ( 'NONE',  ( 65.85249911436491743, 7.562528597612068045E-15, 0.000000000000000000 ) ) ;
#15031 = ORIENTED_EDGE ( 'NONE', *, *, #23948, .T. ) ;
#15032 = ORIENTED_EDGE ( 'NONE', *, *, #19154, .T. ) ;
#15033 = AXIS2_PLACEMENT_3D ( 'NONE', #3817, #11224, #1968 ) ;
#15034 = EDGE_CURVE ( 'NONE', #17358, #13793, #10450, .T. ) ;
#15035 = DIRECTION ( 'NONE',  ( 0.000000000000000000, 0.000000000000000000, 1.000000000000000000 ) ) ;
#15036 = EDGE_LOOP ( 'NONE', ( #15161, #1926 ) ) ;
#15037 = DIRECTION ( 'NONE',  ( 0.000000000000000000, 0.000000000000000000, 1.000000000000000000 ) ) ;
#15038 = AXIS2_PLACEMENT_3D ( 'NONE', #15690, #13886, #19492 ) ;
#15039 = DIRECTION ( 'NONE',  ( -0.000000000000000000, 1.000000000000000000, -0.000000000000000000 ) ) ;
#15040 = CARTESIAN_POINT ( 'NONE',  ( 27.89784171216406961, 41.49349862090490859, -3.000000000000000000 ) ) ;
#15041 = VECTOR ( 'NONE', #12785, 1000.000000000000000 ) ;
#15042 = DIRECTION ( 'NONE',  ( 0.000000000000000000, 0.000000000000000000, 1.000000000000000000 ) ) ;
#15043 = LINE ( 'NONE', #5789, #9139 ) ;
#15044 = EDGE_LOOP ( 'NONE', ( #24005, #8765 ) ) ;
#15045 = CARTESIAN_POINT ( 'NONE',  ( 5.378177448618336243, 9.747164428915397139, 0.000000000000000000 ) ) ;
#15046 = CARTESIAN_POINT ( 'NONE',  ( 40.00000000000000000, 28.80990663662251450, 11.00000000000000000 ) ) ;
#15047 = VERTEX_POINT ( 'NONE', #15833 ) ;
#15048 = ORIENTED_EDGE ( 'NONE', *, *, #8144, .F. ) ;
#15049 = CARTESIAN_POINT ( 'NONE',  ( -5.871322893124554021, 8.081182679343978492, 10.75958914175814130 ) ) ;
#15050 = ORIENTED_EDGE ( 'NONE', *, *, #22303, .T. ) ;
#15051 = EDGE_CURVE ( 'NONE', #22790, #3124, #202, .T. ) ;
#15052 = VECTOR ( 'NONE', #13190, 1000.000000000000000 ) ;
#15053 = PRODUCT_CONTEXT ( 'NONE', #16939, 'mechanical' ) ;
#15054 = ADVANCED_FACE ( 'NONE', ( #22225, #14992 ), #18673, .T. ) ;
#15055 = ORIENTED_EDGE ( 'NONE', *, *, #15735, .F. ) ;
#15056 = ORIENTED_EDGE ( 'NONE', *, *, #14947, .T. ) ;
#15057 = EDGE_CURVE ( 'NONE', #1666, #7729, #2773, .T. ) ;
#15058 = CARTESIAN_POINT ( 'NONE',  ( 23.00000000000000000, 11.58003564732003277, -1.573866785045813010 ) ) ;
#15059 = CARTESIAN_POINT ( 'NONE',  ( -8.680847955711007202, -5.923547351154968927E-13, -7.633165578109188942 ) ) ;
#15060 = ORIENTED_EDGE ( 'NONE', *, *, #8088, .T. ) ;
#15061 = DIRECTION ( 'NONE',  ( -1.000000000000000000, -1.224606353822377258E-16, -0.000000000000000000 ) ) ;
#15062 = DIRECTION ( 'NONE',  ( -1.000000000000000000, 0.000000000000000000, 0.000000000000000000 ) ) ;
#15063 = CARTESIAN_POINT ( 'NONE',  ( -40.66734255040736201, -26.56420859267092283, -3.000000000000000000 ) ) ;
#15064 = ADVANCED_FACE ( 'NONE', ( #19496 ), #6923, .F. ) ;
#15065 = CARTESIAN_POINT ( 'NONE',  ( 1.500000000000001332, 0.000000000000000000, 0.000000000000000000 ) ) ;
#15066 = DIRECTION ( 'NONE',  ( 0.000000000000000000, 0.000000000000000000, -1.000000000000000000 ) ) ;
#15067 = CARTESIAN_POINT ( 'NONE',  ( -34.10000000000000142, -29.50000000000001066, -27.00000000000000000 ) ) ;
#15068 = EDGE_LOOP ( 'NONE', ( #20475, #14056, #7263, #23801 ) ) ;
#15069 = DIRECTION ( 'NONE',  ( -1.000000000000000000, -1.224606353822377258E-16, -0.000000000000000000 ) ) ;
#15070 =( LENGTH_UNIT ( ) NAMED_UNIT ( * ) SI_UNIT ( .MILLI., .METRE. ) );
#15071 = CARTESIAN_POINT ( 'NONE',  ( 15.00000000000000355, 15.50000000000000000, 14.70000000000000284 ) ) ;
#15072 = CARTESIAN_POINT ( 'NONE',  ( 40.66734255040736201, -26.56420859267091217, -3.000000000000000000 ) ) ;
#15073 = CARTESIAN_POINT ( 'NONE',  ( 41.00000000000000000, -4.000000000000015099, 10.49999999999999822 ) ) ;
#15074 = CARTESIAN_POINT ( 'NONE',  ( -8.680847955711200825, 2.820578480813073607, -11.53316557810918752 ) ) ;
#15075 = SURFACE_STYLE_USAGE ( .BOTH. , #9699 ) ;
#15076 = EDGE_LOOP ( 'NONE', ( #14297, #1676 ) ) ;
#15077 = VERTEX_POINT ( 'NONE', #8504 ) ;
#15078 = ORIENTED_EDGE ( 'NONE', *, *, #15339, .T. ) ;
#15079 = EDGE_CURVE ( 'NONE', #16948, #12158, #23586, .T. ) ;
#15080 = AXIS2_PLACEMENT_3D ( 'NONE', #2236, #9658, #2480 ) ;
#15081 = ORIENTED_EDGE ( 'NONE', *, *, #7326, .T. ) ;
#15082 = CARTESIAN_POINT ( 'NONE',  ( 28.27483331787888332, -41.23752903419610050, 27.00000000000000000 ) ) ;
#15083 = VERTEX_POINT ( 'NONE', #4867 ) ;
#15084 = ADVANCED_FACE ( 'NONE', ( #954, #14344 ), #16059, .F. ) ;
#15085 = CARTESIAN_POINT ( 'NONE',  ( 29.00000000000000355, 29.50000000000000000, 27.00000000000000000 ) ) ;
#15086 = EDGE_CURVE ( 'NONE', #12158, #22436, #14231, .T. ) ;
#15087 = AXIS2_PLACEMENT_3D ( 'NONE', #3450, #10752, #14663 ) ;
#15088 = CARTESIAN_POINT ( 'NONE',  ( -31.74999999999995737, 0.000000000000000000, 0.000000000000000000 ) ) ;
#15089 = DIRECTION ( 'NONE',  ( -1.000000000000000000, 0.000000000000000000, 0.000000000000000000 ) ) ;
#15090 = CARTESIAN_POINT ( 'NONE',  ( 73.12522638709218370, -5.000000000000000888, 6.123233995736776143E-16 ) ) ;
#15091 = DIRECTION ( 'NONE',  ( -0.000000000000000000, -0.000000000000000000, -1.000000000000000000 ) ) ;
#15092 = FACE_OUTER_BOUND ( 'NONE', #12700, .T. ) ;
#15093 = ORIENTED_EDGE ( 'NONE', *, *, #1134, .F. ) ;
#15094 = PRODUCT_DEFINITION_SHAPE ( 'NONE', 'NONE',  #24126 ) ;
#15095 = CARTESIAN_POINT ( 'NONE',  ( -41.00000000000000000, -26.23076770084981746, 12.00000000000000000 ) ) ;
#15096 = SURFACE_STYLE_USAGE ( .BOTH. , #16936 ) ;
#15097 = DIRECTION ( 'NONE',  ( 0.000000000000000000, 0.000000000000000000, 1.000000000000000000 ) ) ;
#15098 = CARTESIAN_POINT ( 'NONE',  ( 0.000000000000000000, 0.000000000000000000, 15.50000000000000000 ) ) ;
#15099 = DIRECTION ( 'NONE',  ( 0.000000000000000000, 0.000000000000000000, 1.000000000000000000 ) ) ;
#15100 = EDGE_LOOP ( 'NONE', ( #5302, #15689, #16264, #5501 ) ) ;
#15101 = AXIS2_PLACEMENT_3D ( 'NONE', #12578, #6877, #16489 ) ;
#15102 = ORIENTED_EDGE ( 'NONE', *, *, #963, .T. ) ;
#15103 = EDGE_CURVE ( 'NONE', #14151, #21144, #6447, .T. ) ;
#15104 = EDGE_LOOP ( 'NONE', ( #14690, #18232, #2582, #10465 ) ) ;
#15105 = CARTESIAN_POINT ( 'NONE',  ( -9.500000000000211386, 3.086737114211961064, 8.959589141758140585 ) ) ;
#15106 = ORIENTED_EDGE ( 'NONE', *, *, #8875, .T. ) ;
#15107 = DIRECTION ( 'NONE',  ( 1.000000000000000000, 0.000000000000000000, 0.000000000000000000 ) ) ;
#15108 = EDGE_CURVE ( 'NONE', #5396, #15397, #19861, .T. ) ;
#15109 = DIRECTION ( 'NONE',  ( 0.000000000000000000, -1.000000000000000000, 0.000000000000000000 ) ) ;
#15110 = EDGE_CURVE ( 'NONE', #2102, #7962, #16159, .T. ) ;
#15111 = FACE_OUTER_BOUND ( 'NONE', #10090, .T. ) ;
#15112 = MECHANICAL_DESIGN_GEOMETRIC_PRESENTATION_REPRESENTATION (  '', ( #1889 ), #20600 ) ;
#15113 = CARTESIAN_POINT ( 'NONE',  ( 9.499999999999790390, 3.086737114213260025, -6.159589141758145203 ) ) ;
#15114 = VERTEX_POINT ( 'NONE', #17528 ) ;
#15115 = CARTESIAN_POINT ( 'NONE',  ( -5.762672935462116008, 8.116485190583384579, 11.90304097605235967 ) ) ;
#15116 = ORIENTED_EDGE ( 'NONE', *, *, #9451, .F. ) ;
#15117 = DIRECTION ( 'NONE',  ( -1.000000000000000000, 0.000000000000000000, -0.000000000000000000 ) ) ;
#15118 = CARTESIAN_POINT ( 'NONE',  ( 2.980236203076845669, 8.492341138852641080, 80.60398831450446266 ) ) ;
#15119 = DIRECTION ( 'NONE',  ( 0.000000000000000000, -0.2817325568414366654, 0.9594929736144953702 ) ) ;
#15120 = DIRECTION ( 'NONE',  ( 0.000000000000000000, 0.000000000000000000, 1.000000000000000000 ) ) ;
#15121 = CARTESIAN_POINT ( 'NONE',  ( 0.000000000000000000, -2.110835303355385051, 14.05523051341064722 ) ) ;
#15122 = VECTOR ( 'NONE', #7684, 1000.000000000000000 ) ;
#15123 = CARTESIAN_POINT ( 'NONE',  ( 9.499999999999799272, 3.086737114213245370, -7.306742014460232859 ) ) ;
#15124 = CARTESIAN_POINT ( 'NONE',  ( 0.000000000000000000, 0.000000000000000000, -1.500000000000000000 ) ) ;
#15125 = EDGE_CURVE ( 'NONE', #13276, #19210, #14814, .T. ) ;
#15126 = DIRECTION ( 'NONE',  ( -1.000000000000000000, -1.224606353822377258E-16, -0.000000000000000000 ) ) ;
#15127 = EDGE_LOOP ( 'NONE', ( #18426, #1214 ) ) ;
#15128 = CARTESIAN_POINT ( 'NONE',  ( 5.000000000000000000, 4.685197434473818312, -1.301042606982605321E-15 ) ) ;
#15129 = CARTESIAN_POINT ( 'NONE',  ( 41.00000000000000000, 3.999999999999987121, 9.500000000000000000 ) ) ;
#15130 = DIRECTION ( 'NONE',  ( -0.000000000000000000, -0.000000000000000000, -1.000000000000000000 ) ) ;
#15131 = DIRECTION ( 'NONE',  ( 0.7071067811865292541, 8.659560562354708526E-17, -0.7071067811865658914 ) ) ;
#15132 = FACE_OUTER_BOUND ( 'NONE', #14407, .T. ) ;
#15133 = VERTEX_POINT ( 'NONE', #3490 ) ;
#15134 = EDGE_CURVE ( 'NONE', #47, #20318, #20858, .T. ) ;
#15135 = EDGE_CURVE ( 'NONE', #17527, #22631, #18621, .T. ) ;
#15136 = ORIENTED_EDGE ( 'NONE', *, *, #17180, .F. ) ;
#15137 = ITEM_DEFINED_TRANSFORMATION ( 'NONE', 'NONE', #8817,  #8005 ) ;
#15138 = ORIENTED_EDGE ( 'NONE', *, *, #11948, .T. ) ;
#15139 = DIRECTION ( 'NONE',  ( 0.000000000000000000, 0.000000000000000000, 1.000000000000000000 ) ) ;
#15140 = DIRECTION ( 'NONE',  ( 0.000000000000000000, 0.000000000000000000, 1.000000000000000000 ) ) ;
#15141 = EDGE_LOOP ( 'NONE', ( #12442, #9614, #6768, #19503 ) ) ;
#15142 = EDGE_LOOP ( 'NONE', ( #17126, #9055, #17570, #22219 ) ) ;
#15143 = DIRECTION ( 'NONE',  ( -1.000000000000000000, 0.000000000000000000, 0.000000000000000000 ) ) ;
#15144 = ORIENTED_EDGE ( 'NONE', *, *, #9808, .T. ) ;
#15145 = CARTESIAN_POINT ( 'NONE',  ( -8.103571562645766946, -4.965588994209959139, -3.501545554889576639 ) ) ;
#15146 = ORIENTED_EDGE ( 'NONE', *, *, #6533, .T. ) ;
#15147 = FACE_OUTER_BOUND ( 'NONE', #8266, .T. ) ;
#15148 = CARTESIAN_POINT ( 'NONE',  ( 41.50000000000000000, 28.80990663662250739, 11.00000000000000000 ) ) ;
#15149 = CARTESIAN_POINT ( 'NONE',  ( 3.890962118697714531E-15, 15.50000000000000000, 19.20000000000000995 ) ) ;
#15150 = FACE_OUTER_BOUND ( 'NONE', #16117, .T. ) ;
#15151 = ORIENTED_EDGE ( 'NONE', *, *, #9515, .T. ) ;
#15152 = CYLINDRICAL_SURFACE ( 'NONE', #8321, 6.050000000006050982 ) ;
#15153 = CARTESIAN_POINT ( 'NONE',  ( 41.50000000000000000, 28.80990663662250739, 12.00000000000000000 ) ) ;
#15154 = DIRECTION ( 'NONE',  ( 0.000000000000000000, -0.9096319953545136672, -0.4154150130018965936 ) ) ;
#15155 = ORIENTED_EDGE ( 'NONE', *, *, #2483, .T. ) ;
#15156 = CARTESIAN_POINT ( 'NONE',  ( -2.682529543900285862, 8.255977015246234174, 7.233165578109188587 ) ) ;
#15157 = EDGE_LOOP ( 'NONE', ( #14605, #14684, #11600, #8175 ) ) ;
#15158 = VECTOR ( 'NONE', #14095, 1000.000000000000000 ) ;
#15159 = EDGE_CURVE ( 'NONE', #15532, #20601, #14972, .T. ) ;
#15160 = CARTESIAN_POINT ( 'NONE',  ( -20.84999999999999787, -16.67999999999985050, 13.00000000000000178 ) ) ;
#15161 = ORIENTED_EDGE ( 'NONE', *, *, #12787, .T. ) ;
#15162 = ORIENTED_EDGE ( 'NONE', *, *, #8919, .F. ) ;
#15163 = CARTESIAN_POINT ( 'NONE',  ( -9.500000000000000000, 0.000000000000000000, 12.50000000000000000 ) ) ;
#15164 = CARTESIAN_POINT ( 'NONE',  ( -6.153822176767817416E-13, 9.500000000000000000, -2.559589141758142450 ) ) ;
#15165 = DIRECTION ( 'NONE',  ( 1.000000000000000000, 1.224606353822377258E-16, 0.000000000000000000 ) ) ;
#15166 = VERTEX_POINT ( 'NONE', #11147 ) ;
#15167 = DIRECTION ( 'NONE',  ( -1.000000000000000000, 0.000000000000000000, 0.000000000000000000 ) ) ;
#15168 = DIRECTION ( 'NONE',  ( -1.445602896647339163E-16, 0.000000000000000000, -1.000000000000000000 ) ) ;
#15169 = CARTESIAN_POINT ( 'NONE',  ( -42.00000000000000000, 6.000000000000001776, 11.00000000000000000 ) ) ;
#15170 = CARTESIAN_POINT ( 'NONE',  ( 23.00000000000000000, 3.378881074890309311, 11.18737882312122878 ) ) ;
#15171 = CARTESIAN_POINT ( 'NONE',  ( 39.00000000000000000, -28.80990663662251805, 12.00000000000000000 ) ) ;
#15172 = DIRECTION ( 'NONE',  ( 0.000000000000000000, 0.000000000000000000, 1.000000000000000000 ) ) ;
#15173 = CARTESIAN_POINT ( 'NONE',  ( -40.89823313241237912, 26.41789760203348081, 27.00000000000000000 ) ) ;
#15174 = CONICAL_SURFACE ( 'NONE', #401, 4.172000000000008590, 0.9599310885968742602 ) ;
#15175 = EDGE_CURVE ( 'NONE', #105, #5101, #2200, .T. ) ;
#15176 = ORIENTED_EDGE ( 'NONE', *, *, #7703, .T. ) ;
#15177 = CARTESIAN_POINT ( 'NONE',  ( 39.00000000000000000, 28.80990663662251805, 12.00000000000000000 ) ) ;
#15178 = CARTESIAN_POINT ( 'NONE',  ( -5.976739099259236459E-13, 9.226949318570335734, 2.750781287208490689 ) ) ;
#15179 = CARTESIAN_POINT ( 'NONE',  ( 86.21613547800127719, 7.562528597612068045E-15, 0.000000000000000000 ) ) ;
#15180 = LINE ( 'NONE', #20466, #9502 ) ;
#15181 = DIRECTION ( 'NONE',  ( 1.000000000000000000, 3.469446951953611033E-15, 0.000000000000000000 ) ) ;
#15182 = ADVANCED_FACE ( 'NONE', ( #14455 ), #16762, .F. ) ;
#15183 = DIRECTION ( 'NONE',  ( -0.7071067811865469066, 0.000000000000000000, 0.7071067811865482389 ) ) ;
#15184 = CARTESIAN_POINT ( 'NONE',  ( -1.999999999999997113, -45.00000000000000000, -2.974999999999996092 ) ) ;
#15185 = ORIENTED_EDGE ( 'NONE', *, *, #1233, .T. ) ;
#15186 = ADVANCED_FACE ( 'NONE', ( #20445 ), #16540, .F. ) ;
#15187 = ORIENTED_EDGE ( 'NONE', *, *, #3440, .F. ) ;
#15188 = EDGE_CURVE ( 'NONE', #16945, #4703, #4496, .T. ) ;
#15189 = EDGE_LOOP ( 'NONE', ( #8007, #16560 ) ) ;
#15190 =( LENGTH_UNIT ( ) NAMED_UNIT ( * ) SI_UNIT ( .MILLI., .METRE. ) );
#15191 = AXIS2_PLACEMENT_3D ( 'NONE', #14730, #11047, #21944 ) ;
#15192 = EDGE_LOOP ( 'NONE', ( #9237, #1900, #15146, #12090 ) ) ;
#15193 = CARTESIAN_POINT ( 'NONE',  ( -39.99999999999999289, -27.79189783386527779, 27.00000000000000000 ) ) ;
#15194 = UNCERTAINTY_MEASURE_WITH_UNIT (LENGTH_MEASURE( 1.000000000000000082E-05 ), #10487, 'distance_accuracy_value', 'NONE');
#15195 = CARTESIAN_POINT ( 'NONE',  ( 5.021738411795485746, -7.393327316361921753, 12.50000000000000178 ) ) ;
#15196 = DIRECTION ( 'NONE',  ( 0.000000000000000000, 0.000000000000000000, -1.000000000000000000 ) ) ;
#15197 = CARTESIAN_POINT ( 'NONE',  ( -41.00000000000000000, -6.000000000000000888, 12.00000000000000000 ) ) ;
#15198 = DIRECTION ( 'NONE',  ( 0.000000000000000000, -0.000000000000000000, -1.000000000000000000 ) ) ;
#15199 = CARTESIAN_POINT ( 'NONE',  ( -9.500000000000000000, -6.482511860946779655E-13, 11.05958914175814556 ) ) ;
#15200 = CARTESIAN_POINT ( 'NONE',  ( 0.000000000000000000, -15.23000000000000220, -27.00000000000000000 ) ) ;
#15201 = EDGE_CURVE ( 'NONE', #18612, #23403, #79, .T. ) ;
#15202 = DIRECTION ( 'NONE',  ( -0.000000000000000000, -0.000000000000000000, 1.000000000000000000 ) ) ;
#15203 = CARTESIAN_POINT ( 'NONE',  ( 23.00000000000000000, 0.000000000000000000, 0.000000000000000000 ) ) ;
#15204 = VECTOR ( 'NONE', #10320, 1000.000000000000000 ) ;
#15205 = LINE ( 'NONE', #8024, #2331 ) ;
#15206 = EDGE_CURVE ( 'NONE', #13970, #13300, #9216, .T. ) ;
#15207 = EDGE_LOOP ( 'NONE', ( #13336, #5418 ) ) ;
#15208 = EDGE_CURVE ( 'NONE', #21717, #23772, #22805, .T. ) ;
#15209 = CONICAL_SURFACE ( 'NONE', #22262, 5.025000000000002132, 0.7853981633974482790 ) ;
#15210 = DIRECTION ( 'NONE',  ( 0.000000000000000000, -1.000000000000000000, 0.000000000000000000 ) ) ;
#15211 = VERTEX_POINT ( 'NONE', #18262 ) ;
#15212 = EDGE_LOOP ( 'NONE', ( #6401, #6561, #4961, #6985 ) ) ;
#15213 = CARTESIAN_POINT ( 'NONE',  ( 2.935661446562616295, -9.035036904803758873, 9.659589141758143427 ) ) ;
#15214 = VERTEX_POINT ( 'NONE', #10680 ) ;
#15215 =( NAMED_UNIT ( * ) SI_UNIT ( $, .STERADIAN. ) SOLID_ANGLE_UNIT ( ) );
#15216 = DIRECTION ( 'NONE',  ( 1.000000000000000000, 0.000000000000000000, 0.000000000000000000 ) ) ;
#15217 = CARTESIAN_POINT ( 'NONE',  ( 0.000000000000000000, 0.000000000000000000, 105.0000000000000000 ) ) ;
#15218 = CARTESIAN_POINT ( 'NONE',  ( 74.87477361290781630, 7.420530141404717394E-15, 0.000000000000000000 ) ) ;
#15219 = AXIS2_PLACEMENT_3D ( 'NONE', #22209, #21964, #10723 ) ;
#15220 = CARTESIAN_POINT ( 'NONE',  ( 73.42022815836234884, 5.000000000000025757, 6.123233995736788962E-16 ) ) ;
#15221 = CARTESIAN_POINT ( 'NONE',  ( 23.90000000000000924, -29.50000000000000711, 27.00000000000000000 ) ) ;
#15222 = CIRCLE ( 'NONE', #14089, 1.499999999999994449 ) ;
#15223 = VECTOR ( 'NONE', #4609, 1000.000000000000000 ) ;
#15224 = EDGE_CURVE ( 'NONE', #10152, #19491, #23991, .T. ) ;
#15225 = FACE_OUTER_BOUND ( 'NONE', #19697, .T. ) ;
#15226 = ORIENTED_EDGE ( 'NONE', *, *, #17903, .T. ) ;
#15227 = CYLINDRICAL_SURFACE ( 'NONE', #19566, 18.49999999999999645 ) ;
#15228 = ORIENTED_EDGE ( 'NONE', *, *, #21474, .F. ) ;
#15229 = CARTESIAN_POINT ( 'NONE',  ( -2.468715102574523534, -8.804291563376645868, 12.36424688184530396 ) ) ;
#15230 = DIRECTION ( 'NONE',  ( 1.000000000000000000, 0.000000000000000000, 0.000000000000000000 ) ) ;
#15231 = DIRECTION ( 'NONE',  ( -0.000000000000000000, 1.000000000000000000, -0.000000000000000000 ) ) ;
#15232 = EDGE_CURVE ( 'NONE', #3029, #5970, #12756, .T. ) ;
#15233 = DIRECTION ( 'NONE',  ( -1.000000000000000000, -0.000000000000000000, -0.000000000000000000 ) ) ;
#15234 = EDGE_CURVE ( 'NONE', #15114, #12189, #8758, .T. ) ;
#15235 = CARTESIAN_POINT ( 'NONE',  ( -2.599936666271553509, 8.617022755512742549, 79.49060476457101743 ) ) ;
#15236 = ADVANCED_FACE ( 'NONE', ( #7027 ), #20467, .T. ) ;
#15237 = DIRECTION ( 'NONE',  ( -0.000000000000000000, -0.000000000000000000, -1.000000000000000000 ) ) ;
#15238 = CARTESIAN_POINT ( 'NONE',  ( 0.000000000000000000, 0.000000000000000000, 12.50000000000000000 ) ) ;
#15239 = LINE ( 'NONE', #20897, #13406 ) ;
#15240 = CIRCLE ( 'NONE', #11722, 5.000000000000007994 ) ;
#15241 = ORIENTED_EDGE ( 'NONE', *, *, #1801, .T. ) ;
#15242 = VECTOR ( 'NONE', #18276, 1000.000000000000000 ) ;
#15243 = FACE_OUTER_BOUND ( 'NONE', #18317, .T. ) ;
#15244 = CARTESIAN_POINT ( 'NONE',  ( -6.233975306307045953E-13, 9.127583699786111282, 9.133165578109188942 ) ) ;
#15245 = CIRCLE ( 'NONE', #10592, 4.999999999999997335 ) ;
#15246 = DIRECTION ( 'NONE',  ( 1.000000000000000000, 1.224606353822377258E-16, 0.000000000000000000 ) ) ;
#15247 = DIRECTION ( 'NONE',  ( -0.000000000000000000, -0.000000000000000000, -1.000000000000000000 ) ) ;
#15248 = ORIENTED_EDGE ( 'NONE', *, *, #606, .T. ) ;
#15249 = ORIENTED_EDGE ( 'NONE', *, *, #19924, .T. ) ;
#15250 = ORIENTED_EDGE ( 'NONE', *, *, #23224, .T. ) ;
#15251 = CARTESIAN_POINT ( 'NONE',  ( 80.39795365981946418, 7.562528597612068045E-15, 0.000000000000000000 ) ) ;
#15252 = EDGE_CURVE ( 'NONE', #17567, #12916, #3708, .T. ) ;
#15253 = CARTESIAN_POINT ( 'NONE',  ( 5.871322893123449127, 8.081182679344781405, -9.506742014460231260 ) ) ;
#15254 = ORIENTED_EDGE ( 'NONE', *, *, #1123, .F. ) ;
#15255 = VECTOR ( 'NONE', #13113, 1000.000000000000000 ) ;
#15256 = EDGE_LOOP ( 'NONE', ( #3071, #3193 ) ) ;
#15257 = DIRECTION ( 'NONE',  ( -1.000000000000000000, 0.000000000000000000, 0.000000000000000000 ) ) ;
#15258 = VECTOR ( 'NONE', #23420, 1000.000000000000000 ) ;
#15259 = CARTESIAN_POINT ( 'NONE',  ( -41.49999999999999289, 27.79189783386526358, 27.00000000000000000 ) ) ;
#15260 = AXIS2_PLACEMENT_3D ( 'NONE', #8533, #2689, #6841 ) ;
#15261 = VERTEX_POINT ( 'NONE', #15058 ) ;
#15262 = AXIS2_PLACEMENT_3D ( 'NONE', #1990, #60, #16649 ) ;
#15263 = VECTOR ( 'NONE', #12207, 1000.000000000000000 ) ;
#15264 = ADVANCED_FACE ( 'NONE', ( #9564 ), #2055, .T. ) ;
#15265 = ORIENTED_EDGE ( 'NONE', *, *, #12426, .F. ) ;
#15266 = EDGE_CURVE ( 'NONE', #20691, #6266, #7609, .T. ) ;
#15267 = DIRECTION ( 'NONE',  ( 0.000000000000000000, 0.000000000000000000, 1.000000000000000000 ) ) ;
#15268 = CYLINDRICAL_SURFACE ( 'NONE', #14129, 5.100000000000000533 ) ;
#15269 = CARTESIAN_POINT ( 'NONE',  ( -10.00000000000000000, 0.000000000000000000, 0.000000000000000000 ) ) ;
#15270 = FACE_OUTER_BOUND ( 'NONE', #15068, .T. ) ;
#15271 = ORIENTED_EDGE ( 'NONE', *, *, #12313, .T. ) ;
#15272 = CARTESIAN_POINT ( 'NONE',  ( 65.85249911436491743, 6.123233995736675563E-16, -5.000000000000007994 ) ) ;
#15273 = CARTESIAN_POINT ( 'NONE',  ( -30.68762588338048403, 45.64284848299540442, 0.000000000000000000 ) ) ;
#15274 = FACE_OUTER_BOUND ( 'NONE', #15942, .T. ) ;
#15275 = ORIENTED_EDGE ( 'NONE', *, *, #8736, .F. ) ;
#15276 = ORIENTED_EDGE ( 'NONE', *, *, #16614, .T. ) ;
#15277 = CARTESIAN_POINT ( 'NONE',  ( 5.871322893124553133, -8.081182679343980269, 11.75958914175814485 ) ) ;
#15278 = ORIENTED_EDGE ( 'NONE', *, *, #7300, .T. ) ;
#15279 = AXIS2_PLACEMENT_3D ( 'NONE', #18629, #13126, #14463 ) ;
#15280 = CIRCLE ( 'NONE', #9832, 11.00000000000000711 ) ;
#15281 = AXIS2_PLACEMENT_3D ( 'NONE', #21722, #16326, #3054 ) ;
#15282 = LINE ( 'NONE', #10392, #1757 ) ;
#15283 = AXIS2_PLACEMENT_3D ( 'NONE', #11464, #19169, #18939 ) ;
#15284 = AXIS2_PLACEMENT_3D ( 'NONE', #11308, #14861, #7542 ) ;
#15285 = EDGE_LOOP ( 'NONE', ( #6821, #17988, #9778 ) ) ;
#15286 = EDGE_LOOP ( 'NONE', ( #21167, #8121, #11777, #18559 ) ) ;
#15287 = FACE_OUTER_BOUND ( 'NONE', #23064, .T. ) ;
#15288 = LINE ( 'NONE', #6048, #9593 ) ;
#15289 = CIRCLE ( 'NONE', #2440, 1.500000000000001332 ) ;
#15290 = SHAPE_REPRESENTATION ( 'Pin 4X6', ( #8005 ), #13887 ) ;
#15291 = FACE_OUTER_BOUND ( 'NONE', #3251, .T. ) ;
#15292 = EDGE_CURVE ( 'NONE', #3962, #3370, #15688, .T. ) ;
#15293 = ORIENTED_EDGE ( 'NONE', *, *, #8731, .F. ) ;
#15294 = DIRECTION ( 'NONE',  ( -1.000000000000000000, -0.000000000000000000, -0.000000000000000000 ) ) ;
#15295 = DIRECTION ( 'NONE',  ( 0.000000000000000000, -1.000000000000000000, 0.000000000000000000 ) ) ;
#15296 = DIRECTION ( 'NONE',  ( -0.000000000000000000, -0.000000000000000000, -1.000000000000000000 ) ) ;
#15297 = DIRECTION ( 'NONE',  ( -0.000000000000000000, -0.000000000000000000, -1.000000000000000000 ) ) ;
#15298 = CARTESIAN_POINT ( 'NONE',  ( 83.60204634018053582, 7.420530141404717394E-15, 0.000000000000000000 ) ) ;
#15299 = ORIENTED_EDGE ( 'NONE', *, *, #96, .F. ) ;
#15300 = DIRECTION ( 'NONE',  ( 1.000000000000000000, -6.938893903907232322E-15, 0.000000000000000000 ) ) ;
#15301 = DIRECTION ( 'NONE',  ( -0.000000000000000000, -0.000000000000000000, -1.000000000000000000 ) ) ;
#15302 = AXIS2_PLACEMENT_3D ( 'NONE', #8841, #9509, #5182 ) ;
#15303 = AXIS2_PLACEMENT_3D ( 'NONE', #6696, #3271, #14128 ) ;
#15304 = ORIENTED_EDGE ( 'NONE', *, *, #16535, .F. ) ;
#15305 = CARTESIAN_POINT ( 'NONE',  ( 74.87477361290781630, 7.420530141404717394E-15, 0.000000000000000000 ) ) ;
#15306 = ADVANCED_FACE ( 'NONE', ( #21045 ), #14148, .T. ) ;
#15307 = FACE_OUTER_BOUND ( 'NONE', #1957, .T. ) ;
#15308 = CIRCLE ( 'NONE', #11786, 23.84999999999999432 ) ;
#15309 = DIRECTION ( 'NONE',  ( 1.000000000000000000, 0.000000000000000000, 0.000000000000000000 ) ) ;
#15310 = CIRCLE ( 'NONE', #21583, 4.999999999999997335 ) ;
#15311 = CONICAL_SURFACE ( 'NONE', #22735, 0.7000000000000005107, 0.7853981633974458365 ) ;
#15312 = CARTESIAN_POINT ( 'NONE',  ( 9.500000000000200728, -3.086737114211976607, -5.959589141758144137 ) ) ;
#15313 = CARTESIAN_POINT ( 'NONE',  ( 23.00000000000000000, 8.890849273385601492, 7.584660931657517757 ) ) ;
#15314 = ORIENTED_EDGE ( 'NONE', *, *, #11437, .F. ) ;
#15315 = VECTOR ( 'NONE', #14768, 1000.000000000000114 ) ;
#15316 = DIRECTION ( 'NONE',  ( 1.000000000000000000, 1.224606353822377258E-16, 0.000000000000000000 ) ) ;
#15317 = VERTEX_POINT ( 'NONE', #20681 ) ;
#15318 = ORIENTED_EDGE ( 'NONE', *, *, #16256, .F. ) ;
#15319 = CARTESIAN_POINT ( 'NONE',  ( -5.365059087798939252, -7.384370330707086261, 11.93316557810918965 ) ) ;
#15320 = VERTEX_POINT ( 'NONE', #17388 ) ;
#15321 =( NAMED_UNIT ( * ) SI_UNIT ( $, .STERADIAN. ) SOLID_ANGLE_UNIT ( ) );
#15322 = DIRECTION ( 'NONE',  ( -0.000000000000000000, -0.000000000000000000, 1.000000000000000000 ) ) ;
#15323 = CARTESIAN_POINT ( 'NONE',  ( -7.685661446562381371, 5.583959896777970222, -10.85958914175814449 ) ) ;
#15324 = EDGE_CURVE ( 'NONE', #8771, #22613, #11776, .T. ) ;
#15325 = VECTOR ( 'NONE', #17482, 1000.000000000000000 ) ;
#15326 = AXIS2_PLACEMENT_3D ( 'NONE', #9269, #12481, #1284 ) ;
#15327 = DIRECTION ( 'NONE',  ( -0.000000000000000000, -0.000000000000000000, 1.000000000000000000 ) ) ;
#15328 = CARTESIAN_POINT ( 'NONE',  ( -47.34180362313354351, -6.000000000000002665, 11.00000000000000000 ) ) ;
#15329 = CARTESIAN_POINT ( 'NONE',  ( 7.685661446562381371, -5.583959896777971110, 7.006742014460233037 ) ) ;
#15330 = CARTESIAN_POINT ( 'NONE',  ( 9.499999999999790390, 3.086737114213260025, -5.306742014460231971 ) ) ;
#15331 = EDGE_CURVE ( 'NONE', #8760, #24045, #15289, .T. ) ;
#15332 = AXIS2_PLACEMENT_3D ( 'NONE', #12238, #17240, #21035 ) ;
#15333 = VERTEX_POINT ( 'NONE', #11744 ) ;
#15334 = DIRECTION ( 'NONE',  ( 4.613626265895764052E-16, -1.000000000000000000, 0.000000000000000000 ) ) ;
#15335 = VECTOR ( 'NONE', #3148, 1000.000000000000000 ) ;
#15336 = EDGE_CURVE ( 'NONE', #3116, #9659, #9432, .T. ) ;
#15337 = CARTESIAN_POINT ( 'NONE',  ( 30.32370777929699202, 42.16181938034194587, 0.000000000000000000 ) ) ;
#15338 = CYLINDRICAL_SURFACE ( 'NONE', #21098, 5.000000000000000888 ) ;
#15339 = EDGE_CURVE ( 'NONE', #14877, #19090, #6163, .T. ) ;
#15340 = CARTESIAN_POINT ( 'NONE',  ( 0.000000000000000000, 0.000000000000000000, 53.00000000000000000 ) ) ;
#15341 = CARTESIAN_POINT ( 'NONE',  ( -16.08510323282435550, 6.088885580147183951, -7.295537496892093188 ) ) ;
#15342 = CYLINDRICAL_SURFACE ( 'NONE', #2094, 5.000000000000000888 ) ;
#15343 = ORIENTED_EDGE ( 'NONE', *, *, #7804, .F. ) ;
#15344 =( GEOMETRIC_REPRESENTATION_CONTEXT ( 3 ) GLOBAL_UNCERTAINTY_ASSIGNED_CONTEXT ( ( #7872 ) ) GLOBAL_UNIT_ASSIGNED_CONTEXT ( ( #3623, #7039, #3272 ) ) REPRESENTATION_CONTEXT ( 'NONE', 'WORKASPACE' ) );
#15345 = ORIENTED_EDGE ( 'NONE', *, *, #3936, .T. ) ;
#15346 = AXIS2_PLACEMENT_3D ( 'NONE', #18567, #13163, #1845 ) ;
#15347 = VERTEX_POINT ( 'NONE', #11380 ) ;
#15348 = CARTESIAN_POINT ( 'NONE',  ( -2.935661446561384391, -9.035036904804158553, 11.45958914175814414 ) ) ;
#15349 = CARTESIAN_POINT ( 'NONE',  ( 64.69295543108962931, 7.420530141404717394E-15, 0.000000000000000000 ) ) ;
#15350 = VECTOR ( 'NONE', #1030, 1000.000000000000114 ) ;
#15351 = VERTEX_POINT ( 'NONE', #2261 ) ;
#15352 = CARTESIAN_POINT ( 'NONE',  ( 0.000000000000000000, 0.000000000000000000, 15.50000000000000000 ) ) ;
#15353 = CARTESIAN_POINT ( 'NONE',  ( 0.000000000000000000, -45.00000000000000000, 3.000000000000002665 ) ) ;
#15354 = VECTOR ( 'NONE', #13362, 1000.000000000000000 ) ;
#15355 = CARTESIAN_POINT ( 'NONE',  ( 71.09090909090909349, -4.172000000000000597, 5.616230220889771312E-16 ) ) ;
#15356 = ORIENTED_EDGE ( 'NONE', *, *, #20506, .T. ) ;
#15357 = CARTESIAN_POINT ( 'NONE',  ( 0.000000000000000000, 15.03999999999999915, 27.00000000000000000 ) ) ;
#15358 = ADVANCED_FACE ( 'NONE', ( #22764 ), #17258, .T. ) ;
#15359 = CARTESIAN_POINT ( 'NONE',  ( 9.499999999999996447, 1.163414459189985091E-15, 0.000000000000000000 ) ) ;
#15360 = CARTESIAN_POINT ( 'NONE',  ( 0.000000000000000000, 0.000000000000000000, 0.2999999999999990452 ) ) ;
#15361 = ADVANCED_FACE ( 'NONE', ( #18858 ), #3229, .T. ) ;
#15362 = CIRCLE ( 'NONE', #20448, 5.000000000000007994 ) ;
#15364 = EDGE_CURVE ( 'NONE', #21393, #10212, #17131, .T. ) ;
#15363 = CARTESIAN_POINT ( 'NONE',  ( -5.871322893123450015, -8.081182679344781405, -3.359589141758143160 ) ) ;
#15365 = ORIENTED_EDGE ( 'NONE', *, *, #20141, .T. ) ;
#15366 = CIRCLE ( 'NONE', #23182, 1.000000000000000888 ) ;
#15367 = CARTESIAN_POINT ( 'NONE',  ( 1.999999999999994449, -45.00000000000000000, 3.000000000000002665 ) ) ;
#15368 = ORIENTED_EDGE ( 'NONE', *, *, #15703, .F. ) ;
#15369 = DIRECTION ( 'NONE',  ( -1.000000000000000000, -0.000000000000000000, -0.000000000000000000 ) ) ;
#15370 = CIRCLE ( 'NONE', #7966, 4.057500000000000107 ) ;
#15371 = CARTESIAN_POINT ( 'NONE',  ( -8.866614027893694683, 3.263134433186268613, 12.05545359443210529 ) ) ;
#15372 = DIRECTION ( 'NONE',  ( -0.000000000000000000, 0.000000000000000000, -1.000000000000000000 ) ) ;
#15373 = VECTOR ( 'NONE', #21963, 1000.000000000000000 ) ;
#15374 = FACE_OUTER_BOUND ( 'NONE', #17269, .T. ) ;
#15375 = CARTESIAN_POINT ( 'NONE',  ( -9.999999999999998224, 0.000000000000000000, 0.000000000000000000 ) ) ;
#15376 = LINE ( 'NONE', #21005, #2049 ) ;
#15377 = CARTESIAN_POINT ( 'NONE',  ( -40.00000000000000000, 0.000000000000000000, 0.000000000000000000 ) ) ;
#15378 = VECTOR ( 'NONE', #9318, 1000.000000000000000 ) ;
#15379 = CIRCLE ( 'NONE', #2935, 5.000000000000007994 ) ;
#15380 = CARTESIAN_POINT ( 'NONE',  ( -2.935661446561384391, -9.035036904804158553, -6.606742014460233570 ) ) ;
#15381 = ORIENTED_EDGE ( 'NONE', *, *, #14158, .F. ) ;
#15382 = CARTESIAN_POINT ( 'NONE',  ( 63.23840997654417606, 7.420530141404717394E-15, 0.000000000000000000 ) ) ;
#15383 = CARTESIAN_POINT ( 'NONE',  ( -5.365059087798940141, -7.384370330707086261, 11.93316557810918965 ) ) ;
#15384 = CARTESIAN_POINT ( 'NONE',  ( 27.89784171216407316, -41.49349862090490149, -3.000000000000000000 ) ) ;
#15385 = CARTESIAN_POINT ( 'NONE',  ( -29.00000000000000000, -29.49999999999999645, 12.00000000000000000 ) ) ;
#15386 = ORIENTED_EDGE ( 'NONE', *, *, #2035, .F. ) ;
#15387 = AXIS2_PLACEMENT_3D ( 'NONE', #175, #12840, #16856 ) ;
#15388 = CIRCLE ( 'NONE', #17351, 4.172000000000008590 ) ;
#15389 = ORIENTED_EDGE ( 'NONE', *, *, #16207, .T. ) ;
#15390 = ADVANCED_FACE ( 'NONE', ( #15287 ), #1687, .F. ) ;
#15391 = ORIENTED_EDGE ( 'NONE', *, *, #22501, .F. ) ;
#15392 = DIRECTION ( 'NONE',  ( 0.000000000000000000, 0.000000000000000000, -1.000000000000000000 ) ) ;
#15393 = EDGE_CURVE ( 'NONE', #15853, #11189, #8282, .T. ) ;
#15394 = AXIS2_PLACEMENT_3D ( 'NONE', #5319, #10892, #18359 ) ;
#15395 = VECTOR ( 'NONE', #9141, 1000.000000000000000 ) ;
#15396 = CARTESIAN_POINT ( 'NONE',  ( 9.500000000000209610, -3.086737114211962396, -9.106742014460232681 ) ) ;
#15397 = VERTEX_POINT ( 'NONE', #4219 ) ;
#15398 = VERTEX_POINT ( 'NONE', #19223 ) ;
#15399 = LINE ( 'NONE', #11718, #1624 ) ;
#15400 = DIRECTION ( 'NONE',  ( -0.000000000000000000, -0.000000000000000000, 1.000000000000000000 ) ) ;
#15401 = ORIENTED_EDGE ( 'NONE', *, *, #5537, .T. ) ;
#15402 = CARTESIAN_POINT ( 'NONE',  ( -9.264724873483777046, -2.172114814696820329, -3.499867591578571968 ) ) ;
#15403 = ORIENTED_EDGE ( 'NONE', *, *, #21457, .F. ) ;
#15404 = CIRCLE ( 'NONE', #1074, 15.00000000000000000 ) ;
#15405 = CARTESIAN_POINT ( 'NONE',  ( -30.31394790604173650, 39.41330121100982353, 12.00000000000000000 ) ) ;
#15406 = LINE ( 'NONE', #23107, #22305 ) ;
#15407 = LINE ( 'NONE', #17368, #2453 ) ;
#15408 = AXIS2_PLACEMENT_3D ( 'NONE', #15085, #22550, #5830 ) ;
#15409 = LINE ( 'NONE', #11981, #7571 ) ;
#15410 = EDGE_LOOP ( 'NONE', ( #10532, #1940 ) ) ;
#15411 = DIRECTION ( 'NONE',  ( 0.000000000000000000, 0.000000000000000000, 1.000000000000000000 ) ) ;
#15412 = CYLINDRICAL_SURFACE ( 'NONE', #21974, 4.249999999999996447 ) ;
#15413 = ORIENTED_EDGE ( 'NONE', *, *, #20208, .F. ) ;
#15414 = AXIS2_PLACEMENT_3D ( 'NONE', #14620, #22090, #7298 ) ;
#15415 = AXIS2_PLACEMENT_3D ( 'NONE', #22269, #16291, #8850 ) ;
#15416 = EDGE_LOOP ( 'NONE', ( #10877, #12289, #19281 ) ) ;
#15417 = CARTESIAN_POINT ( 'NONE',  ( 8.680847955711007202, 5.912916378492122225E-13, 6.633165578109188942 ) ) ;
#15418 = EDGE_CURVE ( 'NONE', #13651, #15766, #11629, .T. ) ;
#15419 = ORIENTED_EDGE ( 'NONE', *, *, #17728, .T. ) ;
#15420 = ORIENTED_EDGE ( 'NONE', *, *, #19691, .T. ) ;
#15421 = EDGE_CURVE ( 'NONE', #5924, #6139, #16080, .T. ) ;
#15422 = ORIENTED_EDGE ( 'NONE', *, *, #23743, .T. ) ;
#15423 = ORIENTED_EDGE ( 'NONE', *, *, #10442, .F. ) ;
#15424 = ADVANCED_FACE ( 'NONE', ( #557 ), #7978, .T. ) ;
#15425 = DIRECTION ( 'NONE',  ( 0.000000000000000000, -1.000000000000000000, 0.000000000000000000 ) ) ;
#15426 = CARTESIAN_POINT ( 'NONE',  ( -7.022953521755574080, 5.102474405759713783, -3.433165578109189209 ) ) ;
#15427 = EDGE_CURVE ( 'NONE', #3309, #8068, #16847, .T. ) ;
#15428 = VECTOR ( 'NONE', #2635, 1000.000000000000227 ) ;
#15429 = ADVANCED_FACE ( 'NONE', ( #12569 ), #7124, .T. ) ;
#15430 = CIRCLE ( 'NONE', #652, 19.84999999999999787 ) ;
#15431 = ORIENTED_EDGE ( 'NONE', *, *, #13505, .F. ) ;
#15432 = CARTESIAN_POINT ( 'NONE',  ( 0.000000000000000000, -15.23000000000000220, -27.00000000000000000 ) ) ;
#15433 = DIRECTION ( 'NONE',  ( 0.8571673007021116675, 0.000000000000000000, 0.5150380749100552658 ) ) ;
#15434 = CARTESIAN_POINT ( 'NONE',  ( 61.48886275072855057, 7.562528597612068045E-15, 0.000000000000000000 ) ) ;
#15435 = DIRECTION ( 'NONE',  ( -1.000000000000000000, -4.613626265895764052E-16, 0.000000000000000000 ) ) ;
#15436 = ORIENTED_EDGE ( 'NONE', *, *, #3289, .F. ) ;
#15437 = DIRECTION ( 'NONE',  ( -1.000000000000000000, -0.000000000000000000, -0.000000000000000000 ) ) ;
#15438 = AXIS2_PLACEMENT_3D ( 'NONE', #15217, #619, #19044 ) ;
#15439=STYLED_ITEM('',(#24162),#2885);
#15440 = DIRECTION ( 'NONE',  ( 0.000000000000000000, 0.000000000000000000, -1.000000000000000000 ) ) ;
#15441 = ORIENTED_EDGE ( 'NONE', *, *, #9930, .T. ) ;
#15442 = LINE ( 'NONE', #11896, #12443 ) ;
#15443 = DIRECTION ( 'NONE',  ( -0.000000000000000000, -0.000000000000000000, -1.000000000000000000 ) ) ;
#15444 = DIRECTION ( 'NONE',  ( -1.000000000000000000, 0.000000000000000000, 0.000000000000000000 ) ) ;
#15445 = CARTESIAN_POINT ( 'NONE',  ( -9.499999999999799272, -3.086737114213243593, -5.159589141758141650 ) ) ;
#15446 = CARTESIAN_POINT ( 'NONE',  ( 5.365059087798939252, 7.384370330707087149, -6.933165578109188765 ) ) ;
#15447 = CARTESIAN_POINT ( 'NONE',  ( 40.66734255040735491, -26.56420859267090862, -3.000000000000000000 ) ) ;
#15448 = ORIENTED_EDGE ( 'NONE', *, *, #7404, .F. ) ;
#15449 = EDGE_CURVE ( 'NONE', #3126, #4922, #22031, .T. ) ;
#15450 = ORIENTED_EDGE ( 'NONE', *, *, #4768, .T. ) ;
#15451 = ORIENTED_EDGE ( 'NONE', *, *, #630, .F. ) ;
#15452 = SHAPE_REPRESENTATION_RELATIONSHIP ( 'NONE' , 'NONE' ,  #852, #8130 ) ;
#15453 =( BOUNDED_CURVE ( )  B_SPLINE_CURVE ( 2, ( #8128, #13757, #1089, #15571, #8509, #23034, #21206 ),
 .UNSPECIFIED., .F., .F. ) 
 B_SPLINE_CURVE_WITH_KNOTS ( ( 3, 2, 2, 3 ),
 ( 0.9000000000000000222, 0.9200000000000000400, 0.9399999999999999467, 0.9500000000000000666 ),
 .UNSPECIFIED. ) 
 CURVE ( )  GEOMETRIC_REPRESENTATION_ITEM ( )  RATIONAL_B_SPLINE_CURVE ( ( 1.000000000000000000, 0.9510565162951535312, 1.000000000000000000, 0.9510565162951535312, 1.000000000000000000, 0.9755282581475764880, 0.9755282581475768211 ) ) 
 REPRESENTATION_ITEM ( '' )  );
#15454 = CARTESIAN_POINT ( 'NONE',  ( 0.000000000000000000, 0.000000000000000000, -27.00000000000000000 ) ) ;
#15455 = ORIENTED_EDGE ( 'NONE', *, *, #5572, .F. ) ;
#15456 = EDGE_CURVE ( 'NONE', #3740, #12921, #6753, .T. ) ;
#15457 = DIRECTION ( 'NONE',  ( 4.613626265895763066E-16, 1.000000000000000000, -0.000000000000000000 ) ) ;
#15458 = PRODUCT_DEFINITION_CONTEXT ( 'detailed design', #23974, 'design' ) ;
#15459 = ADVANCED_FACE ( 'NONE', ( #3442 ), #17235, .F. ) ;
#15460 = CARTESIAN_POINT ( 'NONE',  ( 42.00000000000000000, 25.22443390181681622, -3.000000000000000000 ) ) ;
#15461 = CARTESIAN_POINT ( 'NONE',  ( 8.840695694414906214, -0.6121865488561712976, 12.50000000000000000 ) ) ;
#15462 = CARTESIAN_POINT ( 'NONE',  ( 9.500000000000000000, 6.470877716354879437E-13, 7.206742014460234103 ) ) ;
#15463 = ORIENTED_EDGE ( 'NONE', *, *, #18349, .T. ) ;
#15464 = CARTESIAN_POINT ( 'NONE',  ( 8.871028110654306076, 6.042456644462176420E-13, -12.50000000000000000 ) ) ;
#15465 = DIRECTION ( 'NONE',  ( 0.000000000000000000, 1.000000000000000000, 0.000000000000000000 ) ) ;
#15466 = DIRECTION ( 'NONE',  ( 8.659560562354857670E-17, -0.7071067811865536790, 0.7071067811865414665 ) ) ;
#15467 = EDGE_LOOP ( 'NONE', ( #17879, #12781, #21951, #11344 ) ) ;
#15468 = CARTESIAN_POINT ( 'NONE',  ( -31.74999999999995737, 0.000000000000000000, 0.000000000000000000 ) ) ;
#15469 = CYLINDRICAL_SURFACE ( 'NONE', #2030, 1.499999999999994449 ) ;
#15470 = DIRECTION ( 'NONE',  ( 0.000000000000000000, -0.9898214418809341275, 0.1423148382732755957 ) ) ;
#15471 = CYLINDRICAL_SURFACE ( 'NONE', #9497, 5.000000000000000888 ) ;
#15472 = ORIENTED_EDGE ( 'NONE', *, *, #5774, .T. ) ;
#15473 = CARTESIAN_POINT ( 'NONE',  ( -6.233975306307046963E-13, 9.127583699786111282, -7.133165578109187166 ) ) ;
#15474 = ORIENTED_EDGE ( 'NONE', *, *, #8485, .T. ) ;
#15475 = ORIENTED_EDGE ( 'NONE', *, *, #15877, .T. ) ;
#15476 = CARTESIAN_POINT ( 'NONE',  ( 6.999999999999999112, 0.000000000000000000, 0.000000000000000000 ) ) ;
#15477 = DIRECTION ( 'NONE',  ( -0.000000000000000000, -0.000000000000000000, -1.000000000000000000 ) ) ;
#15478 = EDGE_LOOP ( 'NONE', ( #12166, #2997, #16989, #7662, #22254 ) ) ;
#15479 = CARTESIAN_POINT ( 'NONE',  ( -34.00000000000000000, -4.999999999999999112, 10.49999999999999822 ) ) ;
#15480 = DIRECTION ( 'NONE',  ( 1.000000000000000000, 0.000000000000000000, 0.000000000000000000 ) ) ;
#15481 = LINE ( 'NONE', #12054, #17747 ) ;
#15482 = ADVANCED_FACE ( 'NONE', ( #12456 ), #6740, .T. ) ;
#15483 = CARTESIAN_POINT ( 'NONE',  ( 5.998136232247421873, -6.550536670409211837, -12.49999999999999289 ) ) ;
#15484 = DIRECTION ( 'NONE',  ( 1.000000000000000000, 0.000000000000000000, 0.000000000000000000 ) ) ;
#15485 = CARTESIAN_POINT ( 'NONE',  ( -27.89784171216405895, 41.49349862090491570, -1.500000000000000000 ) ) ;
#15486 = CARTESIAN_POINT ( 'NONE',  ( 7.685661446561619314, 5.583959896779020049, -4.259589141758143960 ) ) ;
#15487 = ORIENTED_EDGE ( 'NONE', *, *, #16477, .T. ) ;
#15488 = CARTESIAN_POINT ( 'NONE',  ( 40.00000000000000000, 0.000000000000000000, 12.00000000000000000 ) ) ;
#15489 = VERTEX_POINT ( 'NONE', #8804 ) ;
#15490 = CARTESIAN_POINT ( 'NONE',  ( 0.9852835067608223252, -9.043392810604785836, 12.43634207785451196 ) ) ;
#15491 = FACE_BOUND ( 'NONE', #22368, .T. ) ;
#15492 = DIRECTION ( 'NONE',  ( 0.000000000000000000, 0.000000000000000000, 1.000000000000000000 ) ) ;
#15493 = DIRECTION ( 'NONE',  ( -1.000000000000000000, -0.000000000000000000, -0.000000000000000000 ) ) ;
#15494 = ADVANCED_FACE ( 'NONE', ( #5144 ), #9029, .T. ) ;
#15495 = CARTESIAN_POINT ( 'NONE',  ( 0.000000000000000000, 0.000000000000000000, 12.50000000000000000 ) ) ;
#15496 = CARTESIAN_POINT ( 'NONE',  ( 67.30704456891035647, 5.000000000000015987, 0.000000000000000000 ) ) ;
#15497 = VERTEX_POINT ( 'NONE', #6977 ) ;
#15498 = CARTESIAN_POINT ( 'NONE',  ( -6.822232771736903637E-13, 9.988891130263535700, -5.706742014460234103 ) ) ;
#15499 = ORIENTED_EDGE ( 'NONE', *, *, #11631, .T. ) ;
#15500 = CARTESIAN_POINT ( 'NONE',  ( -28.99999999999998579, -29.50000000000000711, -1.500000000000000000 ) ) ;
#15501 = PRODUCT_DEFINITION_SHAPE ( 'NONE', 'NONE',  #24117 ) ;
#15502 = EDGE_CURVE ( 'NONE', #9321, #16665, #21168, .T. ) ;
#15503 = CARTESIAN_POINT ( 'NONE',  ( 8.680847955711007202, 5.912916378492122225E-13, 6.633165578109188942 ) ) ;
#15504 = VECTOR ( 'NONE', #20422, 1000.000000000000000 ) ;
#15505 = FACE_OUTER_BOUND ( 'NONE', #407, .T. ) ;
#15506 = CARTESIAN_POINT ( 'NONE',  ( 0.000000000000000000, 0.000000000000000000, 0.000000000000000000 ) ) ;
#15507 = EDGE_CURVE ( 'NONE', #16191, #7578, #11384, .T. ) ;
#15508 = VERTEX_POINT ( 'NONE', #10743 ) ;
#15509 = VECTOR ( 'NONE', #3942, 1000.000000000000000 ) ;
#15510 = CONTEXT_DEPENDENT_SHAPE_REPRESENTATION ( #23825, #11790 ) ;
#15511 = ORIENTED_EDGE ( 'NONE', *, *, #21415, .F. ) ;
#15512 = DIRECTION ( 'NONE',  ( 0.000000000000000000, -1.000000000000000000, 0.000000000000000000 ) ) ;
#15513 = CARTESIAN_POINT ( 'NONE',  ( 7.685661446562381371, -5.583959896777971110, -11.00674201446023304 ) ) ;
#15514 = ORIENTED_EDGE ( 'NONE', *, *, #23929, .T. ) ;
#15515 = CLOSED_SHELL ( 'NONE', ( #11918, #23931, #3001, #3369, #14910, #4729, #16764, #10390, #16176, #16697 ) ) ;
#15516 = CARTESIAN_POINT ( 'NONE',  ( -28.00000000000001066, 50.99999999999999289, 0.5000000000000000000 ) ) ;
#15517 = EDGE_LOOP ( 'NONE', ( #22030, #10921, #292, #20982 ) ) ;
#15518 = VERTEX_POINT ( 'NONE', #11883 ) ;
#15519 = DIRECTION ( 'NONE',  ( 0.000000000000000000, 0.000000000000000000, 1.000000000000000000 ) ) ;
#15520 = DIRECTION ( 'NONE',  ( -0.8247505806839219300, 0.5654966663575777819, -2.861428388275804004E-15 ) ) ;
#15521 = CIRCLE ( 'NONE', #13588, 1.499999999999994449 ) ;
#15522 = CARTESIAN_POINT ( 'NONE',  ( 40.49999999999998579, -51.00000000000000711, 12.50000000000000000 ) ) ;
#15523 = ORIENTED_EDGE ( 'NONE', *, *, #17904, .T. ) ;
#15524 = DIRECTION ( 'NONE',  ( -1.000000000000000000, 1.224646799147351482E-16, 0.000000000000000000 ) ) ;
#15525 = EDGE_CURVE ( 'NONE', #2103, #8542, #18214, .T. ) ;
#15526 = DIRECTION ( 'NONE',  ( -0.000000000000000000, -0.000000000000000000, -1.000000000000000000 ) ) ;
#15527 = EDGE_CURVE ( 'NONE', #2131, #10832, #8914, .T. ) ;
#15528 = ORIENTED_EDGE ( 'NONE', *, *, #14084, .F. ) ;
#15529 = ORIENTED_EDGE ( 'NONE', *, *, #22600, .F. ) ;
#15530 = CARTESIAN_POINT ( 'NONE',  ( -9.500000000000000000, -6.482511860946779655E-13, 5.059589141758143782 ) ) ;
#15531 = ORIENTED_EDGE ( 'NONE', *, *, #1696, .T. ) ;
#15532 = VERTEX_POINT ( 'NONE', #2743 ) ;
#15533 = EDGE_LOOP ( 'NONE', ( #21295, #3179 ) ) ;
#15534 = VERTEX_POINT ( 'NONE', #10042 ) ;
#15535 = ORIENTED_EDGE ( 'NONE', *, *, #21970, .F. ) ;
#15536 = DIRECTION ( 'NONE',  ( 0.000000000000000000, 0.000000000000000000, 1.000000000000000000 ) ) ;
#15537 = CARTESIAN_POINT ( 'NONE',  ( 7.022953521754877748, 5.102474405760673903, -6.833165578109188232 ) ) ;
#15538 = CARTESIAN_POINT ( 'NONE',  ( -9.500000000000216716, 3.086737114211953514, 8.106742014460232681 ) ) ;
#15539 = ORIENTED_EDGE ( 'NONE', *, *, #9905, .T. ) ;
#15540 = CARTESIAN_POINT ( 'NONE',  ( 88.54545454545454675, 7.491529369508391930E-15, 0.000000000000000000 ) ) ;
#15541 = DIRECTION ( 'NONE',  ( -1.000000000000000000, 0.000000000000000000, 0.000000000000000000 ) ) ;
#15542 = CARTESIAN_POINT ( 'NONE',  ( 23.85000000000000142, 15.03999999999999737, 2.200000000000000178 ) ) ;
#15543 = PRODUCT_RELATED_PRODUCT_CATEGORY ( 'part', '', ( #16053 ) ) ;
#15544 = DIRECTION ( 'NONE',  ( -1.000000000000000000, 0.000000000000000000, 0.000000000000000000 ) ) ;
#15545 = EDGE_LOOP ( 'NONE', ( #9214, #7573, #15716, #20155 ) ) ;
#15546 = CARTESIAN_POINT ( 'NONE',  ( 0.000000000000000000, 0.000000000000000000, 0.000000000000000000 ) ) ;
#15547 = DIRECTION ( 'NONE',  ( -1.000000000000000000, -1.224606353822377258E-16, -0.000000000000000000 ) ) ;
#15548 = EDGE_CURVE ( 'NONE', #18856, #22492, #2848, .T. ) ;
#15549 = ORIENTED_EDGE ( 'NONE', *, *, #22854, .T. ) ;
#15550 = DIRECTION ( 'NONE',  ( -0.000000000000000000, -1.000000000000000000, -0.000000000000000000 ) ) ;
#15551 = CARTESIAN_POINT ( 'NONE',  ( -5.799656021750657521E-13, 8.953898637140671468, 2.941973432658839371 ) ) ;
#15552 = EDGE_CURVE ( 'NONE', #14710, #9146, #23106, .T. ) ;
#15553 = AXIS2_PLACEMENT_3D ( 'NONE', #19480, #6290, #10056 ) ;
#15554 = DIRECTION ( 'NONE',  ( 1.000000000000000000, 0.000000000000000000, 0.000000000000000000 ) ) ;
#15555 = EDGE_CURVE ( 'NONE', #6915, #7243, #14899, .T. ) ;
#15556 = CARTESIAN_POINT ( 'NONE',  ( -2.682529543900285862, 8.255977015246234174, -9.233165578109188587 ) ) ;
#15557 = ADVANCED_FACE ( 'NONE', ( #10158, #9499 ), #22350, .F. ) ;
#15558 = VERTEX_POINT ( 'NONE', #23938 ) ;
#15559 = CARTESIAN_POINT ( 'NONE',  ( 60.90909090909091361, 4.172000000000015696, 5.109226446042767468E-16 ) ) ;
#15560 = ORIENTED_EDGE ( 'NONE', *, *, #9801, .T. ) ;
#15561 = ORIENTED_EDGE ( 'NONE', *, *, #15885, .F. ) ;
#15562 = CARTESIAN_POINT ( 'NONE',  ( 5.365059087799946447, -7.384370330706356178, 12.33316557810918646 ) ) ;
#15563 = VERTEX_POINT ( 'NONE', #5630 ) ;
#15564 = CARTESIAN_POINT ( 'NONE',  ( 693.7709501539947041, 890.2451952084554705, 1339.731724745927977 ) ) ;
#15565 = CARTESIAN_POINT ( 'NONE',  ( -5.762672935462112456, 8.116485190583386355, -11.90304097605236144 ) ) ;
#15566 = ORIENTED_EDGE ( 'NONE', *, *, #2323, .F. ) ;
#15567 = CARTESIAN_POINT ( 'NONE',  ( -12.50000000000000178, 1.672973214995343413E-15, -2.500000000000000000 ) ) ;
#15568 = CARTESIAN_POINT ( 'NONE',  ( 9.500000000000209610, -3.086737114211962396, -11.95958914175814591 ) ) ;
#15569 = AXIS2_PLACEMENT_3D ( 'NONE', #10113, #8294, #6492 ) ;
#15570 = DIRECTION ( 'NONE',  ( -1.000000000000000000, -0.000000000000000000, -0.000000000000000000 ) ) ;
#15571 = CARTESIAN_POINT ( 'NONE',  ( -5.871322893124554021, 8.081182679343978492, 3.906742014460231616 ) ) ;
#15572 = DIRECTION ( 'NONE',  ( 0.000000000000000000, -0.000000000000000000, -1.000000000000000000 ) ) ;
#15573 = ORIENTED_EDGE ( 'NONE', *, *, #9492, .F. ) ;
#15574 = CARTESIAN_POINT ( 'NONE',  ( 41.00000000000000000, -5.000000000000015099, 11.00000000000000000 ) ) ;
#15575 = DIRECTION ( 'NONE',  ( -1.000000000000000000, -1.224606353822377258E-16, -0.000000000000000000 ) ) ;
#15576 = EDGE_CURVE ( 'NONE', #20318, #13109, #20522, .T. ) ;
#15577 = LINE ( 'NONE', #2551, #3702 ) ;
#15578 = ORIENTED_EDGE ( 'NONE', *, *, #19182, .T. ) ;
#15579 = CARTESIAN_POINT ( 'NONE',  ( 19.85000000000000142, -16.67999999999999616, 13.50000000000000178 ) ) ;
#15580 = DIRECTION ( 'NONE',  ( -1.000000000000000000, 0.000000000000000000, 0.000000000000000000 ) ) ;
#15581 = DIRECTION ( 'NONE',  ( -1.000000000000000000, 0.000000000000000000, 0.000000000000000000 ) ) ;
#15582 = DIRECTION ( 'NONE',  ( -1.000000000000000000, -1.224606353822377258E-16, -0.000000000000000000 ) ) ;
#15583 = ADVANCED_FACE ( 'NONE', ( #5754 ), #18814, .F. ) ;
#15584 = VERTEX_POINT ( 'NONE', #12816 ) ;
#15585 = EDGE_CURVE ( 'NONE', #13330, #11891, #12567, .T. ) ;
#15586 = ORIENTED_EDGE ( 'NONE', *, *, #3298, .T. ) ;
#15587 = VECTOR ( 'NONE', #2823, 1000.000000000000000 ) ;
#15588 = CARTESIAN_POINT ( 'NONE',  ( 88.54545454545454675, 7.491529369508391930E-15, 0.000000000000000000 ) ) ;
#15589 = DIRECTION ( 'NONE',  ( 1.000000000000000000, 0.000000000000000000, 0.000000000000000000 ) ) ;
#15590 = VERTEX_POINT ( 'NONE', #3673 ) ;
#15591 = CARTESIAN_POINT ( 'NONE',  ( 7.022953521755574080, -5.102474405759714671, -12.43316557810918788 ) ) ;
#15592 = DIRECTION ( 'NONE',  ( 0.9160001545545232160, -0.4011779117250717785, -0.000000000000000000 ) ) ;
#15593 = ORIENTED_EDGE ( 'NONE', *, *, #6908, .T. ) ;
#15594 = LINE ( 'NONE', #6709, #10727 ) ;
#15595 = DIRECTION ( 'NONE',  ( -0.000000000000000000, -0.000000000000000000, 1.000000000000000000 ) ) ;
#15596 = CARTESIAN_POINT ( 'NONE',  ( 23.85000000000000497, 15.03999999999999915, -25.00000000000000000 ) ) ;
#15597 = FACE_OUTER_BOUND ( 'NONE', #1421, .T. ) ;
#15598 = CARTESIAN_POINT ( 'NONE',  ( 0.000000000000000000, 0.000000000000000000, 0.9999999999999731326 ) ) ;
#15599 = ORIENTED_EDGE ( 'NONE', *, *, #16508, .F. ) ;
#15600 = CIRCLE ( 'NONE', #40, 8.000000000000003553 ) ;
#15601 = ORIENTED_EDGE ( 'NONE', *, *, #16023, .F. ) ;
#15602 = DIRECTION ( 'NONE',  ( 1.000000000000000000, 0.000000000000000000, 0.000000000000000000 ) ) ;
#15603 = DIRECTION ( 'NONE',  ( -0.000000000000000000, -0.000000000000000000, -1.000000000000000000 ) ) ;
#15604 = DIRECTION ( 'NONE',  ( 1.000000000000000000, 0.000000000000000000, 0.000000000000000000 ) ) ;
#15605 = DIRECTION ( 'NONE',  ( 0.000000000000000000, -1.000000000000000000, 0.000000000000000000 ) ) ;
#15606 = VERTEX_POINT ( 'NONE', #20626 ) ;
#15607 = EDGE_CURVE ( 'NONE', #11723, #10733, #14523, .T. ) ;
#15608 = CARTESIAN_POINT ( 'NONE',  ( -6.822232771736904647E-13, 9.988891130263535700, -7.706742014460232326 ) ) ;
#15609 = CARTESIAN_POINT ( 'NONE',  ( 7.685661446561619314, 5.583959896779020049, 8.259589141758144848 ) ) ;
#15610 = EDGE_CURVE ( 'NONE', #11505, #1470, #14912, .T. ) ;
#15611 = ORIENTED_EDGE ( 'NONE', *, *, #8555, .F. ) ;
#15612 = CARTESIAN_POINT ( 'NONE',  ( 2.935661446561383503, 9.035036904804158553, -5.606742014460233570 ) ) ;
#15613 = ORIENTED_EDGE ( 'NONE', *, *, #8492, .F. ) ;
#15614 = CARTESIAN_POINT ( 'NONE',  ( 23.00000000000000000, 0.000000000000000000, 0.000000000000000000 ) ) ;
#15615 = CARTESIAN_POINT ( 'NONE',  ( 6.222797240145152671E-13, -9.127583699786111282, 12.13316557810918717 ) ) ;
#15616 = CARTESIAN_POINT ( 'NONE',  ( 23.00000000000000000, 0.000000000000000000, 0.000000000000000000 ) ) ;
#15617 = DIRECTION ( 'NONE',  ( 0.000000000000000000, 0.000000000000000000, 1.000000000000000000 ) ) ;
#15618 = CIRCLE ( 'NONE', #7428, 23.85000000000000142 ) ;
#15619 = EDGE_LOOP ( 'NONE', ( #9774, #12729 ) ) ;
#15620 = AXIS2_PLACEMENT_3D ( 'NONE', #2388, #22541, #20832 ) ;
#15621 = ORIENTED_EDGE ( 'NONE', *, *, #5309, .F. ) ;
#15622 = ORIENTED_EDGE ( 'NONE', *, *, #4652, .F. ) ;
#15623 = EDGE_CURVE ( 'NONE', #1878, #12712, #16865, .T. ) ;
#15624 = CARTESIAN_POINT ( 'NONE',  ( 5.871322893124553133, -8.081182679343980269, -12.90674201446023517 ) ) ;
#15625 = ORIENTED_EDGE ( 'NONE', *, *, #7526, .F. ) ;
#15626 = ORIENTED_EDGE ( 'NONE', *, *, #5629, .F. ) ;
#15627 = CARTESIAN_POINT ( 'NONE',  ( -7.751616505663432299, -5.097168108095969430, -12.23076385528166909 ) ) ;
#15628 = EDGE_CURVE ( 'NONE', #9192, #3844, #9157, .T. ) ;
#15629 = CARTESIAN_POINT ( 'NONE',  ( 29.00000000000000355, 29.50000000000000000, 27.00000000000000000 ) ) ;
#15630 = ORIENTED_EDGE ( 'NONE', *, *, #16877, .F. ) ;
#15631 = DIRECTION ( 'NONE',  ( -1.000000000000000000, 0.000000000000000000, 0.000000000000000000 ) ) ;
#15632 = AXIS2_PLACEMENT_3D ( 'NONE', #4634, #6458, #22931 ) ;
#15633 = ADVANCED_FACE ( 'NONE', ( #12930 ), #4839, .T. ) ;
#15634 = VECTOR ( 'NONE', #4907, 1000.000000000000000 ) ;
#15635 = EDGE_LOOP ( 'NONE', ( #4716, #20671, #23645, #9395 ) ) ;
#15636 = DIRECTION ( 'NONE',  ( -1.000000000000000000, -1.224606353822377258E-16, -0.000000000000000000 ) ) ;
#15637 = EDGE_CURVE ( 'NONE', #13648, #12337, #17279, .T. ) ;
#15638 = CARTESIAN_POINT ( 'NONE',  ( 87.96568270381690979, 7.420530141404717394E-15, 0.000000000000000000 ) ) ;
#15639 = VECTOR ( 'NONE', #1989, 1000.000000000000000 ) ;
#15640 = LINE ( 'NONE', #908, #7153 ) ;
#15641 = CARTESIAN_POINT ( 'NONE',  ( 85.63636363636365445, 4.172000000000015696, 5.109226446042767468E-16 ) ) ;
#15642 = ORIENTED_EDGE ( 'NONE', *, *, #2218, .T. ) ;
#15643 = DIRECTION ( 'NONE',  ( -0.000000000000000000, -0.000000000000000000, -1.000000000000000000 ) ) ;
#15644 = CYLINDRICAL_SURFACE ( 'NONE', #10267, 5.100000000000000533 ) ;
#15645 = CARTESIAN_POINT ( 'NONE',  ( -6.822232771736904647E-13, 9.988891130263535700, -4.559589141758142894 ) ) ;
#15646 = ORIENTED_EDGE ( 'NONE', *, *, #17847, .F. ) ;
#15647 = EDGE_LOOP ( 'NONE', ( #9671, #13530, #4461 ) ) ;
#15648 = CARTESIAN_POINT ( 'NONE',  ( -9.500000000000000000, -6.482511860946779655E-13, 7.059589141758143782 ) ) ;
#15649 = VERTEX_POINT ( 'NONE', #2570 ) ;
#15650 = ORIENTED_EDGE ( 'NONE', *, *, #18210, .T. ) ;
#15651 = ORIENTED_EDGE ( 'NONE', *, *, #9722, .T. ) ;
#15652 = AXIS2_PLACEMENT_3D ( 'NONE', #3751, #15069, #5574 ) ;
#15653 = VERTEX_POINT ( 'NONE', #10102 ) ;
#15654 = AXIS2_PLACEMENT_3D ( 'NONE', #15179, #19003, #9695 ) ;
#15655 = ORIENTED_EDGE ( 'NONE', *, *, #21395, .F. ) ;
#15656 = CIRCLE ( 'NONE', #5153, 0.2999999999999999334 ) ;
#15657 = CARTESIAN_POINT ( 'NONE',  ( 0.000000000000000000, 5.823083658124882156, -12.96521604808343398 ) ) ;
#15658 = CARTESIAN_POINT ( 'NONE',  ( 0.3000000000000023204, 0.000000000000000000, 0.000000000000000000 ) ) ;
#15659 = EDGE_CURVE ( 'NONE', #566, #21243, #131, .T. ) ;
#15660 = AXIS2_PLACEMENT_3D ( 'NONE', #19412, #20993, #9734 ) ;
#15661 = AXIS2_PLACEMENT_3D ( 'NONE', #16365, #3207, #21874 ) ;
#15662 = CARTESIAN_POINT ( 'NONE',  ( 0.000000000000000000, 0.000000000000000000, 3.499999999999999556 ) ) ;
#15663 = VERTEX_POINT ( 'NONE', #15359 ) ;
#15664 = CARTESIAN_POINT ( 'NONE',  ( -16.99687406587155891, -7.923972684219721785, 5.245599057861376480 ) ) ;
#15665 = DIRECTION ( 'NONE',  ( -0.000000000000000000, -0.000000000000000000, 1.000000000000000000 ) ) ;
#15666 = CONICAL_SURFACE ( 'NONE', #4800, 4.171999999999999709, 0.7853981633974687071 ) ;
#15667 = CARTESIAN_POINT ( 'NONE',  ( -31.74999999999995737, 6.123233995736767268E-16, -5.000000000000000888 ) ) ;
#15668 = EDGE_CURVE ( 'NONE', #14826, #23772, #19048, .T. ) ;
#15669 = CARTESIAN_POINT ( 'NONE',  ( 0.000000000000000000, 45.00000000000000000, 23.99999999999999645 ) ) ;
#15670 = ORIENTED_EDGE ( 'NONE', *, *, #19608, .T. ) ;
#15671 = DIRECTION ( 'NONE',  ( -1.000000000000000000, 0.000000000000000000, 0.000000000000000000 ) ) ;
#15672 = EDGE_LOOP ( 'NONE', ( #9419, #18881 ) ) ;
#15673 = DIRECTION ( 'NONE',  ( 0.000000000000000000, 0.000000000000000000, 1.000000000000000000 ) ) ;
#15674 = CARTESIAN_POINT ( 'NONE',  ( -0.9830802669677229932, 45.00000000000000000, 0.000000000000000000 ) ) ;
#15675 = CARTESIAN_POINT ( 'NONE',  ( -9.499999999999998224, 1.163414459189985288E-15, 15.50000000000000000 ) ) ;
#15676 = CIRCLE ( 'NONE', #5548, 15.00000000000000000 ) ;
#15677 = DIRECTION ( 'NONE',  ( -0.000000000000000000, -0.000000000000000000, 1.000000000000000000 ) ) ;
#15678 = CARTESIAN_POINT ( 'NONE',  ( 7.022953521754877748, 5.102474405760673903, -4.833165578109188232 ) ) ;
#15679 = VECTOR ( 'NONE', #11681, 1000.000000000000000 ) ;
#15680 = AXIS2_PLACEMENT_3D ( 'NONE', #14856, #11562, #11185 ) ;
#15681 = AXIS2_PLACEMENT_3D ( 'NONE', #10104, #8417, #21838 ) ;
#15682 = AXIS2_PLACEMENT_3D ( 'NONE', #5999, #4051, #22708 ) ;
#15683 = CYLINDRICAL_SURFACE ( 'NONE', #5879, 4.999999999999997335 ) ;
#15684 = ORIENTED_EDGE ( 'NONE', *, *, #11688, .T. ) ;
#15685 = VERTEX_POINT ( 'NONE', #13550 ) ;
#15686 = AXIS2_PLACEMENT_3D ( 'NONE', #17434, #6330, #8029 ) ;
#15687 = CARTESIAN_POINT ( 'NONE',  ( -7.022953521754877748, -5.102474405760673015, 7.833165578109188232 ) ) ;
#15688 = CIRCLE ( 'NONE', #4820, 5.000000000000007994 ) ;
#15689 = ORIENTED_EDGE ( 'NONE', *, *, #7972, .T. ) ;
#15690 = CARTESIAN_POINT ( 'NONE',  ( 693.7818939062881327, 933.4837211537982284, 1344.481724745927977 ) ) ;
#15691 = CARTESIAN_POINT ( 'NONE',  ( 30.68762588338046982, -45.64284848299539732, -1.500000000000000000 ) ) ;
#15692 = ORIENTED_EDGE ( 'NONE', *, *, #9116, .F. ) ;
#15693 = APPLICATION_CONTEXT ( 'automotive_design' ) ;
#15694 = DIRECTION ( 'NONE',  ( -0.000000000000000000, -0.000000000000000000, -1.000000000000000000 ) ) ;
#15695 = DIRECTION ( 'NONE',  ( 0.000000000000000000, 0.000000000000000000, 1.000000000000000000 ) ) ;
#15696 = EDGE_CURVE ( 'NONE', #6073, #21978, #7509, .T. ) ;
#15697 = CARTESIAN_POINT ( 'NONE',  ( -9.500000000000000000, -6.482511860946779655E-13, -10.20674201446023233 ) ) ;
#15699 = AXIS2_PLACEMENT_3D ( 'NONE', #1178, #13868, #934 ) ;
#15698 = CARTESIAN_POINT ( 'NONE',  ( -42.00000000000000711, 26.82133436441678498, 0.000000000000000000 ) ) ;
#15700 = CARTESIAN_POINT ( 'NONE',  ( 2.454813078130514813E-15, -16.67999999999999972, 12.00000000000000000 ) ) ;
#15701 = EDGE_CURVE ( 'NONE', #556, #18108, #21960, .T. ) ;
#15702 = VECTOR ( 'NONE', #12650, 1000.000000000000000 ) ;
#15703 = EDGE_CURVE ( 'NONE', #14530, #5080, #2321, .T. ) ;
#15704 = AXIS2_PLACEMENT_3D ( 'NONE', #10880, #1635, #7120 ) ;
#15705 = ORIENTED_EDGE ( 'NONE', *, *, #1288, .T. ) ;
#15706 = CARTESIAN_POINT ( 'NONE',  ( 1.224646799147353207E-16, -14.96647757894464270, 8.749999999999998224 ) ) ;
#15707 = DIRECTION ( 'NONE',  ( 0.000000000000000000, 0.000000000000000000, 1.000000000000000000 ) ) ;
#15708 = DIRECTION ( 'NONE',  ( 0.000000000000000000, -1.000000000000000000, 0.000000000000000000 ) ) ;
#15709 = CARTESIAN_POINT ( 'NONE',  ( 23.00000000000000000, 0.000000000000000000, 0.000000000000000000 ) ) ;
#15710 = DIRECTION ( 'NONE',  ( 1.000000000000000000, 0.000000000000000000, 0.000000000000000000 ) ) ;
#15711 = CONICAL_SURFACE ( 'NONE', #22739, 5.000000000000007994, 0.9599310885968855844 ) ;
#15712 = CARTESIAN_POINT ( 'NONE',  ( -28.99999999999999645, 29.50000000000000711, -3.000000000000000000 ) ) ;
#15713 = CARTESIAN_POINT ( 'NONE',  ( -41.00000000000000000, 5.000000000000000888, 10.49999999999999822 ) ) ;
#15714 = ORIENTED_EDGE ( 'NONE', *, *, #18961, .F. ) ;
#15715 = CARTESIAN_POINT ( 'NONE',  ( -7.685661446562381371, 5.583959896777970222, -12.00674201446023481 ) ) ;
#15716 = ORIENTED_EDGE ( 'NONE', *, *, #6984, .F. ) ;
#15717 = ORIENTED_EDGE ( 'NONE', *, *, #7469, .T. ) ;
#15718 = VECTOR ( 'NONE', #15603, 1000.000000000000000 ) ;
#15719 = CARTESIAN_POINT ( 'NONE',  ( 7.685661446562381371, -5.583959896777971110, 5.859589141758143604 ) ) ;
#15720 = DIRECTION ( 'NONE',  ( 0.000000000000000000, 1.000000000000000000, 0.000000000000000000 ) ) ;
#15721 = CIRCLE ( 'NONE', #6380, 8.000000000000000000 ) ;
#15722 = ORIENTED_EDGE ( 'NONE', *, *, #1019, .T. ) ;
#15723 = DIRECTION ( 'NONE',  ( -0.000000000000000000, -0.000000000000000000, -1.000000000000000000 ) ) ;
#15724 = EDGE_CURVE ( 'NONE', #555, #15898, #2465, .T. ) ;
#15725 = AXIS2_PLACEMENT_3D ( 'NONE', #82, #3853, #14936 ) ;
#15726 = VECTOR ( 'NONE', #10891, 1000.000000000000000 ) ;
#15727 = DIRECTION ( 'NONE',  ( -1.000000000000000000, -1.224606353822377258E-16, -0.000000000000000000 ) ) ;
#15728 = AXIS2_PLACEMENT_3D ( 'NONE', #14334, #10783, #1541 ) ;
#15729 = CYLINDRICAL_SURFACE ( 'NONE', #7991, 4.499999999999997335 ) ;
#15730 = EDGE_CURVE ( 'NONE', #5799, #6174, #19158, .T. ) ;
#15731 = CARTESIAN_POINT ( 'NONE',  ( 14.67173559926288462, -3.179195828807841018, -8.975010320294694921 ) ) ;
#15732 = DIRECTION ( 'NONE',  ( -1.000000000000000000, 0.000000000000000000, 0.000000000000000000 ) ) ;
#15733 = CARTESIAN_POINT ( 'NONE',  ( 78.36363636363637397, 7.491529369508391930E-15, 0.000000000000000000 ) ) ;
#15734 = ADVANCED_FACE ( 'NONE', ( #6344 ), #13790, .F. ) ;
#15735 = EDGE_CURVE ( 'NONE', #14640, #23460, #1300, .T. ) ;
#15736 = ADVANCED_FACE ( 'NONE', ( #19525 ), #4033, .T. ) ;
#15737 = CARTESIAN_POINT ( 'NONE',  ( 41.73082370883260239, 27.62204025492843940, -3.000000000000000000 ) ) ;
#15738 = ORIENTED_EDGE ( 'NONE', *, *, #16902, .F. ) ;
#15739 = DIRECTION ( 'NONE',  ( 0.000000000000000000, -1.000000000000000000, 0.000000000000000000 ) ) ;
#15740 = VERTEX_POINT ( 'NONE', #15220 ) ;
#15741 = DIRECTION ( 'NONE',  ( 0.000000000000000000, -1.000000000000000000, 0.000000000000000000 ) ) ;
#15742 = DIRECTION ( 'NONE',  ( 1.000000000000000000, 0.000000000000000000, 0.000000000000000000 ) ) ;
#15743 = FACE_OUTER_BOUND ( 'NONE', #14133, .T. ) ;
#15744 = DIRECTION ( 'NONE',  ( -0.000000000000000000, -0.000000000000000000, 1.000000000000000000 ) ) ;
#15745 = AXIS2_PLACEMENT_3D ( 'NONE', #17342, #12070, #19543 ) ;
#15746 = CARTESIAN_POINT ( 'NONE',  ( -9.500000000000000000, -6.482511860946779655E-13, -5.059589141758143782 ) ) ;
#15747 = AXIS2_PLACEMENT_3D ( 'NONE', #5291, #1622, #22716 ) ;
#15748 = ORIENTED_EDGE ( 'NONE', *, *, #1536, .F. ) ;
#15749 = VECTOR ( 'NONE', #10658, 1000.000000000000000 ) ;
#15750 = AXIS2_PLACEMENT_3D ( 'NONE', #23385, #14320, #23626 ) ;
#15751 = CARTESIAN_POINT ( 'NONE',  ( 73.12522638709218370, -5.000000000000000000, 6.123233995736775157E-16 ) ) ;
#15752 = DIRECTION ( 'NONE',  ( -1.000000000000000000, 0.000000000000000000, 0.000000000000000000 ) ) ;
#15753 = ORIENTED_EDGE ( 'NONE', *, *, #1667, .F. ) ;
#15754 = LINE ( 'NONE', #19172, #11829 ) ;
#15755 = AXIS2_PLACEMENT_3D ( 'NONE', #6941, #10698, #8979 ) ;
#15756 = ORIENTED_EDGE ( 'NONE', *, *, #9611, .T. ) ;
#15757 = DIRECTION ( 'NONE',  ( -0.000000000000000000, 0.000000000000000000, 1.000000000000000000 ) ) ;
#15758 = CARTESIAN_POINT ( 'NONE',  ( -5.365059087799948223, 7.384370330706355290, 11.33316557810918646 ) ) ;
#15759 = DIRECTION ( 'NONE',  ( -1.000000000000000000, -1.224606353822377258E-16, -0.000000000000000000 ) ) ;
#15760 = EDGE_CURVE ( 'NONE', #2429, #20548, #494, .T. ) ;
#15761 = CARTESIAN_POINT ( 'NONE',  ( 0.000000000000000000, 0.000000000000000000, 105.0000000000000000 ) ) ;
#15762 = CARTESIAN_POINT ( 'NONE',  ( 83.60204634018053582, -5.000000000000009770, 0.000000000000000000 ) ) ;
#15763 = CARTESIAN_POINT ( 'NONE',  ( -7.685661446561619314, -5.583959896779019161, 5.259589141758143960 ) ) ;
#15764 = AXIS2_PLACEMENT_3D ( 'NONE', #14637, #22108, #3423 ) ;
#15765 = CIRCLE ( 'NONE', #190, 9.000000000000000000 ) ;
#15766 = VERTEX_POINT ( 'NONE', #19662 ) ;
#15767 = ORIENTED_EDGE ( 'NONE', *, *, #8410, .T. ) ;
#15768 = DIRECTION ( 'NONE',  ( 0.000000000000000000, 1.000000000000000000, 0.000000000000000000 ) ) ;
#15769 = EDGE_CURVE ( 'NONE', #20616, #9207, #17670, .T. ) ;
#15770 = CARTESIAN_POINT ( 'NONE',  ( -2.935661446561384391, -9.035036904804158553, -8.606742014460234458 ) ) ;
#15771 = VERTEX_POINT ( 'NONE', #4901 ) ;
#15772 = AXIS2_PLACEMENT_3D ( 'NONE', #19392, #8754, #19762 ) ;
#15773 = VERTEX_POINT ( 'NONE', #23326 ) ;
#15774 = CARTESIAN_POINT ( 'NONE',  ( -7.287171073162196144, -5.717079508223483764, -12.24592425542296148 ) ) ;
#15775 = LINE ( 'NONE', #8453, #5134 ) ;
#15776 = EDGE_LOOP ( 'NONE', ( #1665, #7398, #18544, #20170, #8738 ) ) ;
#15777 = CARTESIAN_POINT ( 'NONE',  ( 23.97500000000000497, 29.50000000000000000, -3.000000000000000000 ) ) ;
#15778 = VERTEX_POINT ( 'NONE', #14032 ) ;
#15779 = CARTESIAN_POINT ( 'NONE',  ( 23.00000000000000000, 0.000000000000000000, 0.000000000000000000 ) ) ;
#15780 = FACE_BOUND ( 'NONE', #22154, .T. ) ;
#15781 = DIRECTION ( 'NONE',  ( 0.000000000000000000, 0.000000000000000000, 1.000000000000000000 ) ) ;
#15782 = LINE ( 'NONE', #15522, #8766 ) ;
#15783 = ORIENTED_EDGE ( 'NONE', *, *, #16256, .T. ) ;
#15784 = CARTESIAN_POINT ( 'NONE',  ( 20.85000000000000497, -15.04000000000000270, 0.000000000000000000 ) ) ;
#15785 = CYLINDRICAL_SURFACE ( 'NONE', #20026, 8.000000000000000000 ) ;
#15786 = CARTESIAN_POINT ( 'NONE',  ( 3.136800900838523098E-15, 111.0000000000000000, 98.99999999999998579 ) ) ;
#15787 = ORIENTED_EDGE ( 'NONE', *, *, #12965, .F. ) ;
#15788 = CIRCLE ( 'NONE', #15387, 6.050000000006050982 ) ;
#15789 = CARTESIAN_POINT ( 'NONE',  ( 7.685661446562381371, -5.583959896777971110, 5.859589141758143604 ) ) ;
#15790 = ORIENTED_EDGE ( 'NONE', *, *, #21885, .T. ) ;
#15791 = EDGE_CURVE ( 'NONE', #16259, #8265, #2074, .T. ) ;
#15792 = ORIENTED_EDGE ( 'NONE', *, *, #22529, .F. ) ;
#15793 = AXIS2_PLACEMENT_3D ( 'NONE', #18402, #14484, #14265 ) ;
#15794 = VECTOR ( 'NONE', #5487, 1000.000000000000000 ) ;
#15795 = AXIS2_PLACEMENT_3D ( 'NONE', #8510, #4746, #15838 ) ;
#15796 = EDGE_LOOP ( 'NONE', ( #18880, #19401 ) ) ;
#15797 = ORIENTED_EDGE ( 'NONE', *, *, #20746, .F. ) ;
#15798 = DIRECTION ( 'NONE',  ( 1.000000000000000000, 6.811450227741984732E-14, 0.000000000000000000 ) ) ;
#15799 = LINE ( 'NONE', #13974, #20905 ) ;
#15800 = ADVANCED_FACE ( 'NONE', ( #19784 ), #15711, .T. ) ;
#15801 = CARTESIAN_POINT ( 'NONE',  ( 71.96568270381689558, 6.123233995736675563E-16, -5.000000000000007994 ) ) ;
#15802 = DIRECTION ( 'NONE',  ( 0.000000000000000000, 0.000000000000000000, 1.000000000000000000 ) ) ;
#15803 = ORIENTED_EDGE ( 'NONE', *, *, #21834, .T. ) ;
#15804 = CARTESIAN_POINT ( 'NONE',  ( 86.51113724927145654, 6.123233995736675563E-16, -5.000000000000007994 ) ) ;
#15805 = CARTESIAN_POINT ( 'NONE',  ( 0.000000000000000000, 45.00000000000000000, 27.00000000000000000 ) ) ;
#15806 = CARTESIAN_POINT ( 'NONE',  ( 39.00000000000000000, 0.000000000000000000, 11.00000000000000000 ) ) ;
#15807 = AXIS2_PLACEMENT_3D ( 'NONE', #2175, #22448, #15089 ) ;
#15808 = FACE_OUTER_BOUND ( 'NONE', #21086, .T. ) ;
#15809 = ORIENTED_EDGE ( 'NONE', *, *, #8778, .T. ) ;
#15810 = CARTESIAN_POINT ( 'NONE',  ( 29.00000000000000000, 29.50000000000000355, 11.50000000000000000 ) ) ;
#15811 = VECTOR ( 'NONE', #11200, 1000.000000000000000 ) ;
#15812 = LINE ( 'NONE', #10173, #20636 ) ;
#15813 = CIRCLE ( 'NONE', #9182, 1.499999999999998668 ) ;
#15814 = CARTESIAN_POINT ( 'NONE',  ( 9.000000000000001776, 1.102182119232617911E-15, 12.50000000000000000 ) ) ;
#15815 = VECTOR ( 'NONE', #16399, 1000.000000000000000 ) ;
#15816 = CARTESIAN_POINT ( 'NONE',  ( 17.59008829125738416, -9.499485695642603034, -0.4958780962348203203 ) ) ;
#15817 = DIRECTION ( 'NONE',  ( -0.000000000000000000, -0.000000000000000000, -1.000000000000000000 ) ) ;
#15818 = CARTESIAN_POINT ( 'NONE',  ( 8.680847955711007202, 5.912916378492122225E-13, -6.633165578109188942 ) ) ;
#15819 = ADVANCED_FACE ( 'NONE', ( #8779 ), #6956, .T. ) ;
#15820 = DIRECTION ( 'NONE',  ( -0.000000000000000000, -0.000000000000000000, -1.000000000000000000 ) ) ;
#15821 = VERTEX_POINT ( 'NONE', #18406 ) ;
#15822 = ORIENTED_EDGE ( 'NONE', *, *, #16647, .T. ) ;
#15823 = ADVANCED_FACE ( 'NONE', ( #16574 ), #5582, .T. ) ;
#15824 = CARTESIAN_POINT ( 'NONE',  ( 8.680847955711199049, -2.820578480813074496, 10.53316557810918752 ) ) ;
#15825 = VECTOR ( 'NONE', #692, 1000.000000000000000 ) ;
#15826 = EDGE_LOOP ( 'NONE', ( #11226, #1361, #1870, #19874 ) ) ;
#15827 = DIRECTION ( 'NONE',  ( -0.9999997925849501978, -0.0006440730211828924606, -3.383173648055380207E-16 ) ) ;
#15828 =( GEOMETRIC_REPRESENTATION_CONTEXT ( 3 ) GLOBAL_UNCERTAINTY_ASSIGNED_CONTEXT ( ( #5947 ) ) GLOBAL_UNIT_ASSIGNED_CONTEXT ( ( #13251, #4503, #15321 ) ) REPRESENTATION_CONTEXT ( 'NONE', 'WORKASPACE' ) );
#15829 = EDGE_CURVE ( 'NONE', #21225, #10767, #16441, .T. ) ;
#15830 = PLANE ( 'NONE',  #21433 ) ;
#15831 = CONICAL_SURFACE ( 'NONE', #14255, 9.725923461386811297, 0.5683018928752935350 ) ;
#15832 = EDGE_CURVE ( 'NONE', #14424, #4806, #9843, .T. ) ;
#15833 = CARTESIAN_POINT ( 'NONE',  ( 20.84999999999999432, -15.04000000000000448, 25.00000000000000000 ) ) ;
#15834 = CARTESIAN_POINT ( 'NONE',  ( 20.85000000000000853, 15.03999999999999915, 27.00000000000000000 ) ) ;
#15835 = AXIS2_PLACEMENT_3D ( 'NONE', #8057, #22598, #5876 ) ;
#15836 = CARTESIAN_POINT ( 'NONE',  ( -2.980262510504976259, 8.492331645729697343, 99.39574783822581594 ) ) ;
#15837 = CARTESIAN_POINT ( 'NONE',  ( 0.000000000000000000, 15.03999999999999915, 25.00000000000000000 ) ) ;
#15838 = DIRECTION ( 'NONE',  ( -1.000000000000000000, 0.000000000000000000, 0.000000000000000000 ) ) ;
#15839 = EDGE_LOOP ( 'NONE', ( #14950, #21919, #12819, #24015, #7188 ) ) ;
#15840 = VERTEX_POINT ( 'NONE', #7301 ) ;
#15841 = DIRECTION ( 'NONE',  ( -1.000000000000000000, -1.224606353822377258E-16, -0.000000000000000000 ) ) ;
#15842 = CARTESIAN_POINT ( 'NONE',  ( 23.00000000000000000, -1.934484387511856252, -14.08058594723508072 ) ) ;
#15843 = ORIENTED_EDGE ( 'NONE', *, *, #20282, .F. ) ;
#15844 = CIRCLE ( 'NONE', #9211, 1.499999999999998002 ) ;
#15845 = FACE_OUTER_BOUND ( 'NONE', #6535, .T. ) ;
#15846 = ORIENTED_EDGE ( 'NONE', *, *, #11294, .T. ) ;
#15847 = DIRECTION ( 'NONE',  ( -1.000000000000000000, -1.224606353822377258E-16, -0.000000000000000000 ) ) ;
#15848 = DIRECTION ( 'NONE',  ( 0.000000000000000000, -1.000000000000000000, 0.000000000000000000 ) ) ;
#15849 = VECTOR ( 'NONE', #17757, 1000.000000000000000 ) ;
#15850 = CARTESIAN_POINT ( 'NONE',  ( 19.85000000000000142, 16.67999999999999972, 14.50000000000000000 ) ) ;
#15851 = ORIENTED_EDGE ( 'NONE', *, *, #12448, .T. ) ;
#15852 = AXIS2_PLACEMENT_3D ( 'NONE', #3161, #12666, #23782 ) ;
#15853 = VERTEX_POINT ( 'NONE', #20604 ) ;
#15854 = CARTESIAN_POINT ( 'NONE',  ( -5.871322893124554021, 8.081182679343978492, 4.759589141758144848 ) ) ;
#15855 = EDGE_CURVE ( 'NONE', #13780, #15663, #14540, .T. ) ;
#15856 = ADVANCED_FACE ( 'NONE', ( #14741 ), #22204, .T. ) ;
#15857 = AXIS2_PLACEMENT_3D ( 'NONE', #4966, #23970, #12376 ) ;
#15858 = ORIENTED_EDGE ( 'NONE', *, *, #7590, .F. ) ;
#15859 =( NAMED_UNIT ( * ) PLANE_ANGLE_UNIT ( ) SI_UNIT ( $, .RADIAN. ) );
#15860 = CARTESIAN_POINT ( 'NONE',  ( 77.48886275072855767, -5.000000000000000000, 6.123233995736775157E-16 ) ) ;
#15861 = CARTESIAN_POINT ( 'NONE',  ( 68.76159002345582394, 7.562528597612068045E-15, 0.000000000000000000 ) ) ;
#15862 = CARTESIAN_POINT ( 'NONE',  ( -6.153822176767817416E-13, 9.500000000000000000, 2.559589141758142894 ) ) ;
#15863 = DIRECTION ( 'NONE',  ( 0.000000000000000000, 0.000000000000000000, -1.000000000000000000 ) ) ;
#15864 = AXIS2_PLACEMENT_3D ( 'NONE', #21856, #3545, #18318 ) ;
#15865 = FACE_OUTER_BOUND ( 'NONE', #4817, .T. ) ;
#15866 = DIRECTION ( 'NONE',  ( 1.445602896647339163E-16, 0.000000000000000000, 1.000000000000000000 ) ) ;
#15867 = CARTESIAN_POINT ( 'NONE',  ( 87.09090909090909349, 7.491529369508391930E-15, 0.000000000000000000 ) ) ;
#15868 = PRODUCT_DEFINITION_SHAPE ( 'NONE', 'NONE',  #17349 ) ;
#15869 = PLANE ( 'NONE',  #8638 ) ;
#15870 = ORIENTED_EDGE ( 'NONE', *, *, #21191, .F. ) ;
#15871 = DIRECTION ( 'NONE',  ( 0.000000000000000000, -1.000000000000000000, 0.000000000000000000 ) ) ;
#15872 = ORIENTED_EDGE ( 'NONE', *, *, #15701, .F. ) ;
#15873 = LINE ( 'NONE', #19533, #18753 ) ;
#15874 = PLANE ( 'NONE',  #9850 ) ;
#15875 = FACE_OUTER_BOUND ( 'NONE', #13381, .T. ) ;
#15876 = CARTESIAN_POINT ( 'NONE',  ( 9.301232020971124115, 6.335487896752474877E-13, 12.19876797902887233 ) ) ;
#15877 = EDGE_CURVE ( 'NONE', #6633, #15077, #5477, .T. ) ;
#15878 = CARTESIAN_POINT ( 'NONE',  ( 31.10231664966676846, -45.36128193761570770, 27.00000000000000000 ) ) ;
#15879 = ORIENTED_EDGE ( 'NONE', *, *, #21860, .F. ) ;
#15880 = EDGE_LOOP ( 'NONE', ( #23608, #16984, #10749, #174, #20556 ) ) ;
#15881 = CARTESIAN_POINT ( 'NONE',  ( -2.935661446562617183, 9.035036904803758873, -6.659589141758144315 ) ) ;
#15882 = ORIENTED_EDGE ( 'NONE', *, *, #12548, .F. ) ;
#15883 = CARTESIAN_POINT ( 'NONE',  ( -5.365059087799948223, 7.384370330706355290, 3.333165578109187344 ) ) ;
#15884 = EDGE_CURVE ( 'NONE', #5796, #12524, #7910, .T. ) ;
#15885 = EDGE_CURVE ( 'NONE', #18820, #704, #10829, .T. ) ;
#15886 = CARTESIAN_POINT ( 'NONE',  ( 2.024999999999999911, 45.00000000000000000, -3.000000000000000000 ) ) ;
#15887 = DIRECTION ( 'NONE',  ( -0.000000000000000000, -0.000000000000000000, -1.000000000000000000 ) ) ;
#15888 = LINE ( 'NONE', #21266, #9040 ) ;
#15889 = CARTESIAN_POINT ( 'NONE',  ( -36.00000000000001421, 50.99999999999999289, 0.000000000000000000 ) ) ;
#15890 =( REPRESENTATION_RELATIONSHIP ('NONE','NONE', #21748, #2851 ) REPRESENTATION_RELATIONSHIP_WITH_TRANSFORMATION ( #22051 )SHAPE_REPRESENTATION_RELATIONSHIP( ) );
#15891 = CARTESIAN_POINT ( 'NONE',  ( 3.934052222107162766, -8.094642247421043990, -12.50000000000000000 ) ) ;
#15892 = ORIENTED_EDGE ( 'NONE', *, *, #9208, .T. ) ;
#15893 = ORIENTED_EDGE ( 'NONE', *, *, #8119, .F. ) ;
#15894 = DIRECTION ( 'NONE',  ( 1.000000000000000000, 0.000000000000000000, 0.000000000000000000 ) ) ;
#15895 = CIRCLE ( 'NONE', #5381, 23.84999999999999432 ) ;
#15896 = CARTESIAN_POINT ( 'NONE',  ( -9.500000000000211386, 3.086737114211961064, -10.95958914175814414 ) ) ;
#15897 = ORIENTED_EDGE ( 'NONE', *, *, #1754, .T. ) ;
#15898 = VERTEX_POINT ( 'NONE', #20486 ) ;
#15899 = CARTESIAN_POINT ( 'NONE',  ( 9.500000000000000000, 1.163414459189985485E-15, -3.499999999999999556 ) ) ;
#15900 = FACE_OUTER_BOUND ( 'NONE', #16337, .T. ) ;
#15901 = ORIENTED_EDGE ( 'NONE', *, *, #7755, .F. ) ;
#15902 = LINE ( 'NONE', #12350, #2255 ) ;
#15903 = EDGE_CURVE ( 'NONE', #4207, #20601, #9086, .T. ) ;
#15904 = ORIENTED_EDGE ( 'NONE', *, *, #6046, .T. ) ;
#15905 = CARTESIAN_POINT ( 'NONE',  ( 62.36363636363636687, 7.491529369508391930E-15, 0.000000000000000000 ) ) ;
#15906 = FACE_OUTER_BOUND ( 'NONE', #23016, .T. ) ;
#15907 = DIRECTION ( 'NONE',  ( -0.000000000000000000, -0.000000000000000000, -1.000000000000000000 ) ) ;
#15908 = ORIENTED_EDGE ( 'NONE', *, *, #17545, .T. ) ;
#15909 = CARTESIAN_POINT ( 'NONE',  ( -0.7000000000000005107, 0.000000000000000000, 4.000000000000000000 ) ) ;
#15910 = DIRECTION ( 'NONE',  ( -0.9160001545545232160, -0.4011779117250717785, 0.000000000000000000 ) ) ;
#15911 = EDGE_CURVE ( 'NONE', #23101, #19750, #18757, .T. ) ;
#15912 = DIRECTION ( 'NONE',  ( 1.000000000000000000, 0.000000000000000000, 0.000000000000000000 ) ) ;
#15913 = EDGE_CURVE ( 'NONE', #21353, #18576, #14625, .T. ) ;
#15914 = AXIS2_PLACEMENT_3D ( 'NONE', #10688, #18159, #7154 ) ;
#15915 = CARTESIAN_POINT ( 'NONE',  ( 7.685661446562381371, -5.583959896777971110, 7.859589141758143604 ) ) ;
#15916 = ORIENTED_EDGE ( 'NONE', *, *, #5953, .F. ) ;
#15917 = ORIENTED_EDGE ( 'NONE', *, *, #1411, .F. ) ;
#15918 = ORIENTED_EDGE ( 'NONE', *, *, #10682, .F. ) ;
#15919 = DIRECTION ( 'NONE',  ( -1.000000000000000000, 0.000000000000000000, 0.000000000000000000 ) ) ;
#15920 = AXIS2_PLACEMENT_3D ( 'NONE', #5443, #11677, #14024 ) ;
#15921 = LINE ( 'NONE', #8580, #21603 ) ;
#15922 = CYLINDRICAL_SURFACE ( 'NONE', #21140, 6.050000000006050982 ) ;
#15923 = ORIENTED_EDGE ( 'NONE', *, *, #7420, .T. ) ;
#15924 = DIRECTION ( 'NONE',  ( -1.000000000000000000, 0.000000000000000000, -0.000000000000000000 ) ) ;
#15925 = CARTESIAN_POINT ( 'NONE',  ( 42.00000000000000000, -4.000000000000015099, 8.500000000000000000 ) ) ;
#15926 = ORIENTED_EDGE ( 'NONE', *, *, #7004, .T. ) ;
#15927 = CARTESIAN_POINT ( 'NONE',  ( -5.871322893123449127, -8.081182679344781405, -8.506742014460233037 ) ) ;
#15928 = CARTESIAN_POINT ( 'NONE',  ( 81.27272727272728048, -4.172000000000000597, 0.000000000000000000 ) ) ;
#15929 = CARTESIAN_POINT ( 'NONE',  ( 7.685661446561619314, 5.583959896779020049, 5.406742014460233392 ) ) ;
#15930 = CARTESIAN_POINT ( 'NONE',  ( 9.500000000000000000, 6.470877716354879437E-13, 4.059589141758143782 ) ) ;
#15931 = CARTESIAN_POINT ( 'NONE',  ( -7.685661446562381371, 5.583959896777970222, 4.859589141758143604 ) ) ;
#15932 = DIRECTION ( 'NONE',  ( 0.000000000000000000, 1.000000000000000000, 0.000000000000000000 ) ) ;
#15933 = DIRECTION ( 'NONE',  ( 1.000000000000000000, 0.000000000000000000, 0.000000000000000000 ) ) ;
#15934 = CARTESIAN_POINT ( 'NONE',  ( 15.00000000000000000, 6.781880092842756171E-15, 9.499999999999987566 ) ) ;
#15935 = CARTESIAN_POINT ( 'NONE',  ( -8.680847955710813579, -2.820578480814257549, -7.733165578109188587 ) ) ;
#15936 = AXIS2_PLACEMENT_3D ( 'NONE', #15121, #4418, #18938 ) ;
#15937 = EDGE_CURVE ( 'NONE', #2256, #17414, #3882, .T. ) ;
#15938 = ORIENTED_EDGE ( 'NONE', *, *, #5753, .T. ) ;
#15939 = CARTESIAN_POINT ( 'NONE',  ( 5.000000000000000000, 0.000000000000000000, 0.000000000000000000 ) ) ;
#15940 = VERTEX_POINT ( 'NONE', #1826 ) ;
#15941 = CARTESIAN_POINT ( 'NONE',  ( 2.682529543900284974, -8.255977015246234174, 4.233165578109187699 ) ) ;
#15942 = EDGE_LOOP ( 'NONE', ( #21017, #6350, #1740, #15151 ) ) ;
#15943 = CARTESIAN_POINT ( 'NONE',  ( 722.7818939062881327, 917.9837211537981148, 1368.981724745928204 ) ) ;
#15944 = CARTESIAN_POINT ( 'NONE',  ( 9.500000000000000000, 6.470877716354879437E-13, -11.20674201446023410 ) ) ;
#15945 = ORIENTED_EDGE ( 'NONE', *, *, #3940, .F. ) ;
#15946 = DIRECTION ( 'NONE',  ( -0.000000000000000000, 0.000000000000000000, -1.000000000000000000 ) ) ;
#15947 = CARTESIAN_POINT ( 'NONE',  ( -7.685661446561619314, -5.583959896779019161, -5.259589141758143960 ) ) ;
#15948 = CARTESIAN_POINT ( 'NONE',  ( 1.982719576835328512, 8.780034855501286373, 101.2598540750001774 ) ) ;
#15949 = DIRECTION ( 'NONE',  ( 1.000000000000000000, 6.811450227741984732E-14, -0.000000000000000000 ) ) ;
#15950 = FACE_OUTER_BOUND ( 'NONE', #11910, .T. ) ;
#15951 = ADVANCED_FACE ( 'NONE', ( #1930 ), #12209, .T. ) ;
#15952 = CARTESIAN_POINT ( 'NONE',  ( 0.9999999999999986677, 0.000000000000000000, 0.000000000000000000 ) ) ;
#15953 = AXIS2_PLACEMENT_3D ( 'NONE', #12126, #21058, #19369 ) ;
#15954 = ADVANCED_FACE ( 'NONE', ( #11177 ), #18654, .T. ) ;
#15955 = CARTESIAN_POINT ( 'NONE',  ( 83.60204634018053582, 6.123233995736675563E-16, -5.000000000000007994 ) ) ;
#15956 = DIRECTION ( 'NONE',  ( 0.000000000000000000, 1.000000000000000000, 0.000000000000000000 ) ) ;
#15957 = VERTEX_POINT ( 'NONE', #113 ) ;
#15958 = DIRECTION ( 'NONE',  ( -1.000000000000000000, -0.000000000000000000, -0.000000000000000000 ) ) ;
#15959 = CARTESIAN_POINT ( 'NONE',  ( 8.616390364324422180, 78.23814058202225397, 0.000000000000000000 ) ) ;
#15960 = SHAPE_REPRESENTATION ( 'socket head cap screw_iso_ISO 4762 M10 x 80 - 32S', ( #8005 ), #651 ) ;
#15961 = EDGE_CURVE ( 'NONE', #21357, #1010, #4429, .T. ) ;
#15962 = CARTESIAN_POINT ( 'NONE',  ( 9.500000000000000000, 6.470877716354879437E-13, 5.206742014460234103 ) ) ;
#15963 = VERTEX_POINT ( 'NONE', #7522 ) ;
#15964 = CARTESIAN_POINT ( 'NONE',  ( 5.365059087799946447, -7.384370330706356178, -4.333165578109189120 ) ) ;
#15965 = EDGE_LOOP ( 'NONE', ( #10349, #7417, #15005, #3446 ) ) ;
#15966 = EDGE_LOOP ( 'NONE', ( #23380, #21253, #22884, #8496 ) ) ;
#15967 = CARTESIAN_POINT ( 'NONE',  ( -2.935661446562617183, 9.035036904803758873, 4.659589141758143427 ) ) ;
#15968 = CARTESIAN_POINT ( 'NONE',  ( 5.871322893123449127, 8.081182679344781405, 7.506742014460233037 ) ) ;
#15969 = VERTEX_POINT ( 'NONE', #14968 ) ;
#15970 = CIRCLE ( 'NONE', #22166, 5.000000000000007994 ) ;
#15971 =( NAMED_UNIT ( * ) SI_UNIT ( $, .STERADIAN. ) SOLID_ANGLE_UNIT ( ) );
#15972 = CIRCLE ( 'NONE', #22999, 1.000000000000000000 ) ;
#15973 = CARTESIAN_POINT ( 'NONE',  ( 18.49999999999999645, -15.23000000000000043, -27.00000000000000000 ) ) ;
#15974 = FACE_OUTER_BOUND ( 'NONE', #9777, .T. ) ;
#15975 = DIRECTION ( 'NONE',  ( 0.000000000000000000, -1.000000000000000000, 0.000000000000000000 ) ) ;
#15976 = CARTESIAN_POINT ( 'NONE',  ( 23.00000000000000000, -2.110835303355385051, 14.05523051341064722 ) ) ;
#15977 = CARTESIAN_POINT ( 'NONE',  ( 20.85000000000000497, 15.03999999999999737, 0.000000000000000000 ) ) ;
#15978 = ORIENTED_EDGE ( 'NONE', *, *, #8247, .F. ) ;
#15979 = DIRECTION ( 'NONE',  ( -1.000000000000000000, 0.000000000000000000, 0.000000000000000000 ) ) ;
#15980 = EDGE_CURVE ( 'NONE', #4813, #3733, #23728, .T. ) ;
#15981 = EDGE_CURVE ( 'NONE', #16254, #15685, #18063, .T. ) ;
#15982 = ORIENTED_EDGE ( 'NONE', *, *, #17384, .F. ) ;
#15983 = LINE ( 'NONE', #3064, #3944 ) ;
#15984 = SURFACE_STYLE_USAGE ( .BOTH. , #12193 ) ;
#15985 = DIRECTION ( 'NONE',  ( -0.000000000000000000, -0.000000000000000000, 1.000000000000000000 ) ) ;
#15986 = FACE_OUTER_BOUND ( 'NONE', #18846, .T. ) ;
#15987 = CARTESIAN_POINT ( 'NONE',  ( 30.44534269664590553, -40.40463133211081015, 12.00000000000000000 ) ) ;
#15988 = ORIENTED_EDGE ( 'NONE', *, *, #1019, .F. ) ;
#15989 = DIRECTION ( 'NONE',  ( -1.000000000000000000, -1.224606353822377258E-16, -0.000000000000000000 ) ) ;
#15990 = VERTEX_POINT ( 'NONE', #22664 ) ;
#15991 = CARTESIAN_POINT ( 'NONE',  ( -7.685661446562381371, 5.583959896777970222, -6.859589141758143604 ) ) ;
#15992 = ORIENTED_EDGE ( 'NONE', *, *, #8485, .F. ) ;
#15993 = DIRECTION ( 'NONE',  ( -1.000000000000000000, -1.224606353822377258E-16, -0.000000000000000000 ) ) ;
#15994 = DIRECTION ( 'NONE',  ( -1.000000000000000000, -0.000000000000000000, -0.000000000000000000 ) ) ;
#15995 = LINE ( 'NONE', #16352, #23571 ) ;
#15996 = DIRECTION ( 'NONE',  ( -0.8428161139095668997, 6.591069075708646964E-17, -0.5382016333442104505 ) ) ;
#15997 = CARTESIAN_POINT ( 'NONE',  ( 40.66734255040738333, 26.56420859267091217, -3.000000000000000000 ) ) ;
#15998 = CARTESIAN_POINT ( 'NONE',  ( 39.99999999999999289, 29.50000000000000000, -27.00000000000000000 ) ) ;
#16000 = ORIENTED_EDGE ( 'NONE', *, *, #22096, .T. ) ;
#15999 = VECTOR ( 'NONE', #12015, 1000.000000000000000 ) ;
#16001 = FACE_OUTER_BOUND ( 'NONE', #8300, .T. ) ;
#16002 = CARTESIAN_POINT ( 'NONE',  ( 9.500000000000209610, -3.086737114211962396, -5.106742014460234458 ) ) ;
#16003 = EDGE_LOOP ( 'NONE', ( #13481, #9931, #195, #2133 ) ) ;
#16004 = ORIENTED_EDGE ( 'NONE', *, *, #2787, .F. ) ;
#16005 = CARTESIAN_POINT ( 'NONE',  ( -40.89823313241237912, 26.41789760203348081, -27.00000000000000000 ) ) ;
#16006 = ADVANCED_FACE ( 'NONE', ( #5949 ), #2659, .T. ) ;
#16007 = ADVANCED_FACE ( 'NONE', ( #2406 ), #11915, .F. ) ;
#16008 = VERTEX_POINT ( 'NONE', #11781 ) ;
#16009 = ADVANCED_BREP_SHAPE_REPRESENTATION ( '', ( #18330, #8005 ), #19339 ) ;
#16010 = EDGE_LOOP ( 'NONE', ( #21506, #16406, #7882, #16156 ) ) ;
#16011 = CARTESIAN_POINT ( 'NONE',  ( 84.76159002345582394, -5.000000000000000000, 6.123233995736775157E-16 ) ) ;
#16012 = CARTESIAN_POINT ( 'NONE',  ( -29.00000000000000000, 29.49999999999999645, 11.50000000000000000 ) ) ;
#16013 = CARTESIAN_POINT ( 'NONE',  ( 0.000000000000000000, -14.80154252341788279, -10.02147513732838036 ) ) ;
#16014 = CARTESIAN_POINT ( 'NONE',  ( 9.090423977855502713, 6.191897047423500831E-13, -12.34637735993366725 ) ) ;
#16015 = FACE_OUTER_BOUND ( 'NONE', #3951, .T. ) ;
#16016 = CONICAL_SURFACE ( 'NONE', #2771, 9.725923461386811297, 0.5683018928752935350 ) ;
#16017 = VERTEX_POINT ( 'NONE', #17163 ) ;
#16018 = CARTESIAN_POINT ( 'NONE',  ( -6.153822176767817416E-13, 9.500000000000000000, -2.559589141758142894 ) ) ;
#16019 = CARTESIAN_POINT ( 'NONE',  ( -39.99999999999999289, 29.50000000000000000, -27.00000000000000000 ) ) ;
#16020 = DIRECTION ( 'NONE',  ( -0.5735764363510517105, -0.8191520442889879128, 0.000000000000000000 ) ) ;
#16021 = AXIS2_PLACEMENT_3D ( 'NONE', #3621, #18275, #5345 ) ;
#16022 = CARTESIAN_POINT ( 'NONE',  ( -5.871322893123450015, -8.081182679344781405, 9.359589141758146269 ) ) ;
#16023 = EDGE_CURVE ( 'NONE', #1549, #5954, #3248, .T. ) ;
#16024 = ORIENTED_EDGE ( 'NONE', *, *, #21560, .T. ) ;
#16025 = CARTESIAN_POINT ( 'NONE',  ( 0.000000000000000000, -45.00000000000000000, -2.974999999999996092 ) ) ;
#16026 = DIRECTION ( 'NONE',  ( -0.5735764363510517105, -0.8191520442889879128, 0.000000000000000000 ) ) ;
#16027 = LINE ( 'NONE', #8582, #7499 ) ;
#16028 = CIRCLE ( 'NONE', #8210, 11.00000000000000355 ) ;
#16029 = EDGE_LOOP ( 'NONE', ( #4570, #17908, #5828, #6442 ) ) ;
#16030 = CARTESIAN_POINT ( 'NONE',  ( -17.57797814737053699, -9.461914562436920306, 0.9781177603712988278 ) ) ;
#16031 = CARTESIAN_POINT ( 'NONE',  ( 0.000000000000000000, 15.03999999999999737, 2.200000000000000178 ) ) ;
#16032 = EDGE_CURVE ( 'NONE', #19051, #8084, #23869, .T. ) ;
#16033 = CONICAL_SURFACE ( 'NONE', #22278, 5.025000000000002132, 0.7853981633974482790 ) ;
#16034 = ADVANCED_FACE ( 'NONE', ( #20966 ), #19019, .F. ) ;
#16035 = PLANE ( 'NONE',  #12040 ) ;
#16036 = CIRCLE ( 'NONE', #2398, 1.499999999999994449 ) ;
#16037 = EDGE_LOOP ( 'NONE', ( #1844, #5216, #18632, #12864 ) ) ;
#16038 = CARTESIAN_POINT ( 'NONE',  ( 15.00000000000000000, 5.618453542512190434E-15, -9.499999999999987566 ) ) ;
#16039 = CARTESIAN_POINT ( 'NONE',  ( 21.85000000000000497, 0.000000000000000000, 12.00000000000000000 ) ) ;
#16040 = DIRECTION ( 'NONE',  ( 0.000000000000000000, 0.000000000000000000, 1.000000000000000000 ) ) ;
#16041 = CARTESIAN_POINT ( 'NONE',  ( -10.00000000000000000, 0.000000000000000000, 0.000000000000000000 ) ) ;
#16042 = DIRECTION ( 'NONE',  ( 1.000000000000000000, 0.000000000000000000, 0.000000000000000000 ) ) ;
#16043 = CARTESIAN_POINT ( 'NONE',  ( 17.38700629636781869, -8.908123924593978060, -3.336041480784311286 ) ) ;
#16044 = CARTESIAN_POINT ( 'NONE',  ( 14.79227890392045097, 2.568991289487080110, 9.169086800441901275 ) ) ;
#16045 = CARTESIAN_POINT ( 'NONE',  ( -42.00000000000000000, 25.22443390181683043, -3.000000000000000000 ) ) ;
#16046 = ORIENTED_EDGE ( 'NONE', *, *, #21279, .T. ) ;
#16047 = DIRECTION ( 'NONE',  ( 1.000000000000000000, 0.000000000000000000, 0.000000000000000000 ) ) ;
#16048 = ORIENTED_EDGE ( 'NONE', *, *, #18298, .T. ) ;
#16049 = CIRCLE ( 'NONE', #5139, 1.000000000000000888 ) ;
#16050 = AXIS2_PLACEMENT_3D ( 'NONE', #6667, #10665, #16286 ) ;
#16051 = CARTESIAN_POINT ( 'NONE',  ( -7.022953521755574080, 5.102474405759713783, 7.433165578109188765 ) ) ;
#16052 = AXIS2_PLACEMENT_3D ( 'NONE', #4286, #2078, #11454 ) ;
#16053 = PRODUCT ( 'spur gear_am_Metric - Spur gear 2.75M 11T 20PA 23FW ---S11N75H50L18N', 'spur gear_am_Metric - Spur gear 2.75M 11T 20PA 23FW ---S11N75H50L18N', '', ( #12987 ) ) ;
#16054 = VECTOR ( 'NONE', #23198, 1000.000000000000000 ) ;
#16055 = VERTEX_POINT ( 'NONE', #2174 ) ;
#16056 = ADVANCED_FACE ( 'NONE', ( #4252 ), #8011, .F. ) ;
#16057 = DIRECTION ( 'NONE',  ( 1.000000000000000000, 0.000000000000000000, 0.000000000000000000 ) ) ;
#16058 = EDGE_LOOP ( 'NONE', ( #5906, #22231, #16773, #5505 ) ) ;
#16059 = PLANE ( 'NONE',  #17732 ) ;
#16060 = CARTESIAN_POINT ( 'NONE',  ( 7.685661446561619314, 5.583959896779020049, -4.259589141758143960 ) ) ;
#16061 = CARTESIAN_POINT ( 'NONE',  ( -6.153822176767817416E-13, 9.500000000000000000, 3.499999999999999556 ) ) ;
#16062 = CARTESIAN_POINT ( 'NONE',  ( 0.000000000000000000, 5.823083658124710738, 12.96521604808350503 ) ) ;
#16063 = CARTESIAN_POINT ( 'NONE',  ( -34.00000000000000000, 4.999999999999999112, 11.00000000000000000 ) ) ;
#16064 = EDGE_CURVE ( 'NONE', #18515, #12252, #18853, .T. ) ;
#16065 = ORIENTED_EDGE ( 'NONE', *, *, #17053, .F. ) ;
#16066 = CARTESIAN_POINT ( 'NONE',  ( 6.250000000000000000, 10.82531754730548279, 2.500000000000000000 ) ) ;
#16067 = AXIS2_PLACEMENT_3D ( 'NONE', #20826, #13366, #7851 ) ;
#16068 = VECTOR ( 'NONE', #8551, 1000.000000000000000 ) ;
#16069 = LINE ( 'NONE', #21214, #6433 ) ;
#16070 = VECTOR ( 'NONE', #21217, 1000.000000000000000 ) ;
#16071 = DIRECTION ( 'NONE',  ( 1.000000000000000000, 0.000000000000000000, 0.000000000000000000 ) ) ;
#16072 = PLANE ( 'NONE',  #11348 ) ;
#16073 = CIRCLE ( 'NONE', #19986, 11.00000000000000711 ) ;
#16074 = CARTESIAN_POINT ( 'NONE',  ( 0.000000000000000000, -7.812991839788872461, 16.07708877602009068 ) ) ;
#16075 = AXIS2_PLACEMENT_3D ( 'NONE', #12655, #3275, #18392 ) ;
#16076 = VECTOR ( 'NONE', #23346, 1000.000000000000000 ) ;
#16077 = CARTESIAN_POINT ( 'NONE',  ( 63.23840997654417606, 7.420530141404717394E-15, 0.000000000000000000 ) ) ;
#16078 = ORIENTED_EDGE ( 'NONE', *, *, #6558, .F. ) ;
#16079 = CARTESIAN_POINT ( 'NONE',  ( -2.682529543900285862, 8.255977015246234174, -3.233165578109188587 ) ) ;
#16080 = CIRCLE ( 'NONE', #7890, 17.25000000000000000 ) ;
#16081 = EDGE_LOOP ( 'NONE', ( #17952, #18454, #16973, #9533 ) ) ;
#16082 = ORIENTED_EDGE ( 'NONE', *, *, #2239, .T. ) ;
#16083 = CARTESIAN_POINT ( 'NONE',  ( 9.500000000000000000, 6.470877716354879437E-13, 13.20674201446023410 ) ) ;
#16084 = CARTESIAN_POINT ( 'NONE',  ( 9.500000000000000000, 6.470877716354879437E-13, 9.206742014460234103 ) ) ;
#16085 = VERTEX_POINT ( 'NONE', #17419 ) ;
#16086 = FACE_OUTER_BOUND ( 'NONE', #15104, .T. ) ;
#16087 = CARTESIAN_POINT ( 'NONE',  ( 9.500000000000000000, 6.470877716354879437E-13, -4.059589141758143782 ) ) ;
#16088 = CIRCLE ( 'NONE', #20005, 5.000000000000007994 ) ;
#16089 = ADVANCED_FACE ( 'NONE', ( #2292 ), #717, .T. ) ;
#16090 = CONICAL_SURFACE ( 'NONE', #11785, 2.024999999999999911, 0.7853981633974743692 ) ;
#16091 = CARTESIAN_POINT ( 'NONE',  ( 9.000000000000000000, 1.102182119232617714E-15, 51.99999999999998579 ) ) ;
#16092 = CARTESIAN_POINT ( 'NONE',  ( -34.00000000000000000, 5.999999999999999112, 11.00000000000000000 ) ) ;
#16093 = AXIS2_PLACEMENT_3D ( 'NONE', #16273, #23734, #7001 ) ;
#16094 = CIRCLE ( 'NONE', #19216, 20.85000000000000497 ) ;
#16095 = VERTEX_POINT ( 'NONE', #12285 ) ;
#16096 = CIRCLE ( 'NONE', #4008, 11.24716442891539714 ) ;
#16097 = DIRECTION ( 'NONE',  ( -1.000000000000000000, 0.000000000000000000, 0.000000000000000000 ) ) ;
#16098 = DIRECTION ( 'NONE',  ( -1.000000000000000000, 0.000000000000000000, 0.000000000000000000 ) ) ;
#16099 = EDGE_CURVE ( 'NONE', #20120, #13548, #2891, .T. ) ;
#16100 = CARTESIAN_POINT ( 'NONE',  ( 0.000000000000000000, -45.00000000000000000, 0.000000000000000000 ) ) ;
#16101 = EDGE_CURVE ( 'NONE', #23000, #6922, #5659, .T. ) ;
#16102 =( BOUNDED_CURVE ( )  B_SPLINE_CURVE ( 3, ( #16779, #2155, #9585, #7285 ),
 .UNSPECIFIED., .F., .T. ) 
 B_SPLINE_CURVE_WITH_KNOTS ( ( 4, 4 ),
 ( 4.712388980384689674, 6.283185307179586232 ),
 .UNSPECIFIED. ) 
 CURVE ( )  GEOMETRIC_REPRESENTATION_ITEM ( )  RATIONAL_B_SPLINE_CURVE ( ( 1.000000000000000000, 0.8047378541243649375, 0.8047378541243649375, 1.000000000000000000 ) ) 
 REPRESENTATION_ITEM ( '' )  );
#16103 = VERTEX_POINT ( 'NONE', #6572 ) ;
#16104 = ORIENTED_EDGE ( 'NONE', *, *, #5300, .F. ) ;
#16105 = LINE ( 'NONE', #2944, #8607 ) ;
#16106 = DIRECTION ( 'NONE',  ( -0.000000000000000000, -0.000000000000000000, -1.000000000000000000 ) ) ;
#16107 = CARTESIAN_POINT ( 'NONE',  ( -8.534735993385114128, 4.219016916012935603, -3.499350572060046183 ) ) ;
#16108 = CARTESIAN_POINT ( 'NONE',  ( 23.85000000000000497, 15.03999999999999915, 25.00000000000000000 ) ) ;
#16109 = AXIS2_PLACEMENT_3D ( 'NONE', #635, #4660, #6114 ) ;
#16110 = DIRECTION ( 'NONE',  ( 0.000000000000000000, 0.000000000000000000, -1.000000000000000000 ) ) ;
#16111 = ORIENTED_EDGE ( 'NONE', *, *, #20537, .T. ) ;
#16112 = DIRECTION ( 'NONE',  ( -1.000000000000000000, 0.000000000000000000, 0.000000000000000000 ) ) ;
#16113 = AXIS2_PLACEMENT_3D ( 'NONE', #15153, #17117, #14701 ) ;
#16114 = ORIENTED_EDGE ( 'NONE', *, *, #13955, .F. ) ;
#16115 = CARTESIAN_POINT ( 'NONE',  ( -28.73477696352898292, -42.73830357953205805, 0.000000000000000000 ) ) ;
#16116 = AXIS2_PLACEMENT_3D ( 'NONE', #23733, #7000, #19836 ) ;
#16117 = EDGE_LOOP ( 'NONE', ( #1792, #5589, #13843, #9119, #12753 ) ) ;
#16118 = VECTOR ( 'NONE', #11617, 1000.000000000000000 ) ;
#16119 = CARTESIAN_POINT ( 'NONE',  ( 6.222797240145152671E-13, -9.127583699786111282, 4.133165578109187166 ) ) ;
#16120 = VECTOR ( 'NONE', #19849, 1000.000000000000000 ) ;
#16121 = EDGE_CURVE ( 'NONE', #16017, #16103, #23526, .T. ) ;
#16122 = CONICAL_SURFACE ( 'NONE', #18472, 9.499999999999996447, 0.7853981633974482790 ) ;
#16123 = ORIENTED_EDGE ( 'NONE', *, *, #96, .T. ) ;
#16124 = DIRECTION ( 'NONE',  ( -0.000000000000000000, 0.000000000000000000, -1.000000000000000000 ) ) ;
#16125 = FACE_OUTER_BOUND ( 'NONE', #19585, .T. ) ;
#16126 = EDGE_CURVE ( 'NONE', #10574, #14984, #19660, .T. ) ;
#16127 = FACE_OUTER_BOUND ( 'NONE', #9418, .T. ) ;
#16128 = ORIENTED_EDGE ( 'NONE', *, *, #3129, .F. ) ;
#16129 = PLANE ( 'NONE',  #3738 ) ;
#16130 = CIRCLE ( 'NONE', #4458, 8.000000000000000000 ) ;
#16131 = CARTESIAN_POINT ( 'NONE',  ( -5.871322893123450015, -8.081182679344781405, -4.506742014460231260 ) ) ;
#16132 = EDGE_LOOP ( 'NONE', ( #10296, #15904, #12501, #3 ) ) ;
#16133 = VECTOR ( 'NONE', #5854, 1000.000000000000000 ) ;
#16134 = VERTEX_POINT ( 'NONE', #21697 ) ;
#16135 = CARTESIAN_POINT ( 'NONE',  ( -35.99999999999993605, -60.00000000000000000, 12.50000000000000000 ) ) ;
#16136 = AXIS2_PLACEMENT_3D ( 'NONE', #22881, #15411, #10027 ) ;
#16137 = AXIS2_PLACEMENT_3D ( 'NONE', #10997, #16641, #7358 ) ;
#16138 = CARTESIAN_POINT ( 'NONE',  ( -31.74999999999995737, 6.123233995736767268E-16, -5.000000000000000888 ) ) ;
#16139 = AXIS2_PLACEMENT_3D ( 'NONE', #3044, #19510, #23178 ) ;
#16140 = ORIENTED_EDGE ( 'NONE', *, *, #18777, .F. ) ;
#16141 = CARTESIAN_POINT ( 'NONE',  ( 2.935661446562616295, -9.035036904803758873, -3.659589141758142983 ) ) ;
#16142 = CARTESIAN_POINT ( 'NONE',  ( 18.49999999999999645, -15.23000000000000043, 27.00000000000000000 ) ) ;
#16143 = CARTESIAN_POINT ( 'NONE',  ( 69.63636363636364024, 4.172000000000015696, 5.109226446042767468E-16 ) ) ;
#16144 = ORIENTED_EDGE ( 'NONE', *, *, #7350, .T. ) ;
#16145 = DIRECTION ( 'NONE',  ( 0.000000000000000000, -1.000000000000000000, 0.000000000000000000 ) ) ;
#16146 = CARTESIAN_POINT ( 'NONE',  ( -9.500000000000202505, 3.086737114211975275, -4.959589141758144137 ) ) ;
#16147 = EDGE_CURVE ( 'NONE', #9633, #13492, #12347, .T. ) ;
#16148 = LINE ( 'NONE', #8695, #2788 ) ;
#16149 = CIRCLE ( 'NONE', #9891, 8.999999999999994671 ) ;
#16150 = AXIS2_PLACEMENT_3D ( 'NONE', #3429, #21493, #8546 ) ;
#16151 = EDGE_CURVE ( 'NONE', #8356, #21663, #18022, .T. ) ;
#16152 = EDGE_CURVE ( 'NONE', #1786, #11339, #16195, .T. ) ;
#16153 = AXIS2_PLACEMENT_3D ( 'NONE', #13231, #2379, #7617 ) ;
#16154 = ORIENTED_EDGE ( 'NONE', *, *, #14548, .T. ) ;
#16155 = AXIS2_PLACEMENT_3D ( 'NONE', #968, #6692, #2913 ) ;
#16156 = ORIENTED_EDGE ( 'NONE', *, *, #7725, .T. ) ;
#16157 = ORIENTED_EDGE ( 'NONE', *, *, #21696, .F. ) ;
#16158 = CARTESIAN_POINT ( 'NONE',  ( -31.74999999999995737, 0.000000000000000000, 0.000000000000000000 ) ) ;
#16159 = CIRCLE ( 'NONE', #4899, 1.000000000000000888 ) ;
#16160 = DIRECTION ( 'NONE',  ( -1.000000000000000000, 0.000000000000000000, 0.000000000000000000 ) ) ;
#16161 = CARTESIAN_POINT ( 'NONE',  ( 41.50000000000000000, 28.80990663662250739, 12.00000000000000000 ) ) ;
#16162 = ORIENTED_EDGE ( 'NONE', *, *, #14840, .T. ) ;
#16163 = CARTESIAN_POINT ( 'NONE',  ( -16.19099482616364583, -6.271157271432198144, -7.149633965064782437 ) ) ;
#16164 = DIRECTION ( 'NONE',  ( 0.000000000000000000, -1.000000000000000000, 0.000000000000000000 ) ) ;
#16165 = VERTEX_POINT ( 'NONE', #10332 ) ;
#16166 = DIRECTION ( 'NONE',  ( -1.000000000000000000, 0.000000000000000000, 0.000000000000000000 ) ) ;
#16167 = CARTESIAN_POINT ( 'NONE',  ( 2.935661446562616295, -9.035036904803758873, 7.659589141758144315 ) ) ;
#16168 = AXIS2_PLACEMENT_3D ( 'NONE', #4538, #11945, #19411 ) ;
#16169 = CIRCLE ( 'NONE', #14982, 9.500000000000000000 ) ;
#16170 = FACE_BOUND ( 'NONE', #5657, .T. ) ;
#16171 = CARTESIAN_POINT ( 'NONE',  ( -23.89999999999999858, -29.50000000000001066, 27.00000000000000000 ) ) ;
#16172 = DIRECTION ( 'NONE',  ( -0.000000000000000000, 0.000000000000000000, 1.000000000000000000 ) ) ;
#16173 = AXIS2_PLACEMENT_3D ( 'NONE', #8015, #13172, #20629 ) ;
#16174 = PRODUCT_DEFINITION ( 'UNKNOWN', '', #13094, #15458 ) ;
#16175 = CARTESIAN_POINT ( 'NONE',  ( 17.38971744193258573, -8.915620082851736683, 3.315798060087240096 ) ) ;
#16176 = ADVANCED_FACE ( 'NONE', ( #12505 ), #16122, .F. ) ;
#16177 = VECTOR ( 'NONE', #20253, 1000.000000000000000 ) ;
#16178 = CARTESIAN_POINT ( 'NONE',  ( 29.00000000000000000, -29.50000000000000355, 0.000000000000000000 ) ) ;
#16179 = DIRECTION ( 'NONE',  ( 1.000000000000000000, 0.000000000000000000, 0.000000000000000000 ) ) ;
#16180 = EDGE_CURVE ( 'NONE', #4092, #17720, #957, .T. ) ;
#16181 = AXIS2_PLACEMENT_3D ( 'NONE', #5380, #23576, #8790 ) ;
#16182 = ORIENTED_EDGE ( 'NONE', *, *, #13958, .F. ) ;
#16183 = CARTESIAN_POINT ( 'NONE',  ( -6.233975306307046963E-13, 9.127583699786111282, 11.13316557810918894 ) ) ;
#16184 =( GEOMETRIC_REPRESENTATION_CONTEXT ( 3 ) GLOBAL_UNCERTAINTY_ASSIGNED_CONTEXT ( ( #22551 ) ) GLOBAL_UNIT_ASSIGNED_CONTEXT ( ( #5601, #1827, #20606 ) ) REPRESENTATION_CONTEXT ( 'NONE', 'WORKASPACE' ) );
#16185 = VERTEX_POINT ( 'NONE', #1088 ) ;
#16186 = CARTESIAN_POINT ( 'NONE',  ( 6.222797240145152671E-13, -9.127583699786111282, 4.133165578109187166 ) ) ;
#16187 = EDGE_CURVE ( 'NONE', #5468, #2036, #18625, .T. ) ;
#16188 = ADVANCED_FACE ( 'NONE', ( #16413 ), #8965, .T. ) ;
#16189 = CARTESIAN_POINT ( 'NONE',  ( 693.7818939062879053, 903.9837211537983421, 1275.781724745928614 ) ) ;
#16190 = CARTESIAN_POINT ( 'NONE',  ( 63.81818181818181301, 7.491529369508391930E-15, 0.000000000000000000 ) ) ;
#16191 = VERTEX_POINT ( 'NONE', #12869 ) ;
#16192 = CARTESIAN_POINT ( 'NONE',  ( 5.000000000000000000, 3.513898075855366177, 2.028749999999999609 ) ) ;
#16193 = CARTESIAN_POINT ( 'NONE',  ( 9.500000000000000000, 6.470877716354879437E-13, -6.059589141758143782 ) ) ;
#16194 = CIRCLE ( 'NONE', #22441, 23.85000000000000497 ) ;
#16195 = LINE ( 'NONE', #5088, #6792 ) ;
#16196 = CARTESIAN_POINT ( 'NONE',  ( 0.000000000000000000, 0.000000000000000000, 0.000000000000000000 ) ) ;
#16197 = FACE_OUTER_BOUND ( 'NONE', #12724, .T. ) ;
#16198 = VECTOR ( 'NONE', #17626, 1000.000000000000000 ) ;
#16199 = CARTESIAN_POINT ( 'NONE',  ( 79.81818181818181301, 7.491529369508391930E-15, 0.000000000000000000 ) ) ;
#16200 = VECTOR ( 'NONE', #6400, 1000.000000000000000 ) ;
#16201 = CYLINDRICAL_SURFACE ( 'NONE', #2836, 1.999999999999994449 ) ;
#16202 = DIRECTION ( 'NONE',  ( -1.000000000000000000, 0.000000000000000000, 0.000000000000000000 ) ) ;
#16203 = DIRECTION ( 'NONE',  ( 4.613626265895763066E-16, 1.000000000000000000, -0.000000000000000000 ) ) ;
#16204 = DIRECTION ( 'NONE',  ( 0.5735764363510424957, 0.8191520442889943521, 0.000000000000000000 ) ) ;
#16205 = DIRECTION ( 'NONE',  ( -0.000000000000000000, 0.000000000000000000, 1.000000000000000000 ) ) ;
#16206 = CARTESIAN_POINT ( 'NONE',  ( 16.68233279685676251, 7.225448002938849257, 6.184784653374919117 ) ) ;
#16207 = EDGE_CURVE ( 'NONE', #10216, #19750, #23996, .T. ) ;
#16208 = CARTESIAN_POINT ( 'NONE',  ( 0.000000000000000000, 0.000000000000000000, 15.50000000000000000 ) ) ;
#16209 = EDGE_LOOP ( 'NONE', ( #8677, #2359 ) ) ;
#16210 = DIRECTION ( 'NONE',  ( 1.000000000000000000, 0.000000000000000000, -0.000000000000000000 ) ) ;
#16211 = VECTOR ( 'NONE', #15949, 1000.000000000000000 ) ;
#16212 = DIRECTION ( 'NONE',  ( 1.000000000000000000, 0.000000000000000000, 0.000000000000000000 ) ) ;
#16213 = ORIENTED_EDGE ( 'NONE', *, *, #12283, .F. ) ;
#16214 = CIRCLE ( 'NONE', #12302, 5.000000000000007994 ) ;
#16215 = ORIENTED_EDGE ( 'NONE', *, *, #11117, .T. ) ;
#16216 = CARTESIAN_POINT ( 'NONE',  ( -7.685661446561619314, -5.583959896779019161, 12.40674201446023339 ) ) ;
#16217 = CARTESIAN_POINT ( 'NONE',  ( -5.871322893123450015, -8.081182679344781405, 6.506742014460233925 ) ) ;
#16218 = EDGE_CURVE ( 'NONE', #7831, #5160, #3666, .T. ) ;
#16220 = EDGE_CURVE ( 'NONE', #10011, #12080, #22364, .T. ) ;
#16219 = CONICAL_SURFACE ( 'NONE', #11913, 2.024999999999999911, 0.7853981633974743692 ) ;
#16221 = ORIENTED_EDGE ( 'NONE', *, *, #22450, .F. ) ;
#16222 = CARTESIAN_POINT ( 'NONE',  ( 2.220446049250313081E-13, -5.551115123125782702E-14, 38.00000000000003553 ) ) ;
#16223 = VECTOR ( 'NONE', #24092, 1000.000000000000000 ) ;
#16224 = CYLINDRICAL_SURFACE ( 'NONE', #15852, 5.000000000000000888 ) ;
#16225 = DIRECTION ( 'NONE',  ( 0.7071067811865500152, 8.659560562354902043E-17, 0.7071067811865450192 ) ) ;
#16226 = CARTESIAN_POINT ( 'NONE',  ( -24.75000000000000000, 29.50000000000000000, -3.000000000000000000 ) ) ;
#16227 = VECTOR ( 'NONE', #11032, 1000.000000000000000 ) ;
#16228 = PRODUCT_DEFINITION_FORMATION_WITH_SPECIFIED_SOURCE ( 'ANY', '', #3416, .NOT_KNOWN. ) ;
#16229 = ORIENTED_EDGE ( 'NONE', *, *, #18033, .F. ) ;
#16230 = CONICAL_SURFACE ( 'NONE', #3761, 5.000000000000007994, 0.9599310885968855844 ) ;
#16231 = VERTEX_POINT ( 'NONE', #18734 ) ;
#16232 = FACE_BOUND ( 'NONE', #2922, .T. ) ;
#16233 = CARTESIAN_POINT ( 'NONE',  ( -9.500000053420693646, 0.6115953479451512464, -3.501506748078538678 ) ) ;
#16234 = LINE ( 'NONE', #12800, #20428 ) ;
#16235 = CONICAL_SURFACE ( 'NONE', #18952, 1.024999999999999911, 0.7853981633974396193 ) ;
#16236 = LINE ( 'NONE', #21846, #5457 ) ;
#16237 = CARTESIAN_POINT ( 'NONE',  ( 23.00000000000000000, 10.59264252385236738, 4.936618945406631376 ) ) ;
#16238 = ORIENTED_EDGE ( 'NONE', *, *, #23696, .T. ) ;
#16239 = DIRECTION ( 'NONE',  ( -0.000000000000000000, -1.000000000000000000, -0.000000000000000000 ) ) ;
#16240 = VERTEX_POINT ( 'NONE', #5700 ) ;
#16241 = CARTESIAN_POINT ( 'NONE',  ( -40.89823313241237912, -26.41789760203349502, -27.00000000000000000 ) ) ;
#16242 = TOROIDAL_SURFACE ( 'NONE', #3371, 2.000000000000000000, 1.000000000000000000 ) ;
#16243 = EDGE_CURVE ( 'NONE', #891, #19544, #10275, .T. ) ;
#16244 = VERTEX_POINT ( 'NONE', #13121 ) ;
#16245 = FACE_OUTER_BOUND ( 'NONE', #21043, .T. ) ;
#16246 = CARTESIAN_POINT ( 'NONE',  ( -1.504652183083727168, 9.499999999999904077, -2.610843423304989308 ) ) ;
#16247 = DIRECTION ( 'NONE',  ( -1.000000000000000000, -0.000000000000000000, 0.000000000000000000 ) ) ;
#16248 =( BOUNDED_CURVE ( )  B_SPLINE_CURVE ( 2, ( #1533, #8948, #16390, #20530, #7009, #3803, #22484, #18933, #5071, #3916, #3232 ),
 .UNSPECIFIED., .F., .T. ) 
 B_SPLINE_CURVE_WITH_KNOTS ( ( 3, 2, 2, 2, 2, 3 ),
 ( 0.7000000000000000666, 0.7200000000000000844, 0.7400000000000001021, 0.7600000000000000089, 0.7800000000000000266, 0.8000000000000000444 ),
 .UNSPECIFIED. ) 
 CURVE ( )  GEOMETRIC_REPRESENTATION_ITEM ( )  RATIONAL_B_SPLINE_CURVE ( ( 0.9999999999999997780, 0.9510565162951537532, 1.000000000000000000, 0.9510565162951535312, 1.000000000000000000, 0.9510565162951535312, 1.000000000000000000, 0.9510565162951535312, 1.000000000000000000, 0.9510565162951535312, 1.000000000000000000 ) ) 
 REPRESENTATION_ITEM ( '' )  );
#16249 = DIRECTION ( 'NONE',  ( -1.000000000000000000, 0.000000000000000000, 0.000000000000000000 ) ) ;
#16250 = B_SPLINE_CURVE_WITH_KNOTS ( 'NONE', 3,
 ( #16654, #21905, #9206, #5544, #9078, #23851, #11137, #20089 ),
 .UNSPECIFIED., .F., .F.,
 ( 4, 2, 2, 4 ),
 ( 0.003892319173193285655, 0.004864202078960310274, 0.005836084984727334460, 0.007779850796261383698 ),
 .UNSPECIFIED. ) ;
#16251 = DIRECTION ( 'NONE',  ( -1.000000000000000000, 0.000000000000000000, 0.000000000000000000 ) ) ;
#16252 = CARTESIAN_POINT ( 'NONE',  ( -7.685661446562381371, 5.583959896777970222, -4.006742014460233925 ) ) ;
#16253 = ORIENTED_EDGE ( 'NONE', *, *, #13853, .T. ) ;
#16254 = VERTEX_POINT ( 'NONE', #2013 ) ;
#16255 = LINE ( 'NONE', #2546, #2539 ) ;
#16256 = EDGE_CURVE ( 'NONE', #18301, #12468, #2090, .T. ) ;
#16257 = CARTESIAN_POINT ( 'NONE',  ( 11.50000000000000000, 17.02535186363812514, -5.445458559198938175 ) ) ;
#16258 = EDGE_CURVE ( 'NONE', #22631, #721, #9437, .T. ) ;
#16259 = VERTEX_POINT ( 'NONE', #18506 ) ;
#16260 = PRODUCT_DEFINITION_SHAPE ( 'NONE', 'NONE',  #24111 ) ;
#16261 = CARTESIAN_POINT ( 'NONE',  ( 5.871322893124551356, -8.081182679343980269, -3.759589141758144404 ) ) ;
#16262 = EDGE_CURVE ( 'NONE', #14695, #14839, #5204, .T. ) ;
#16263 = FACE_OUTER_BOUND ( 'NONE', #5529, .T. ) ;
#16264 = ORIENTED_EDGE ( 'NONE', *, *, #12675, .T. ) ;
#16265 = DIRECTION ( 'NONE',  ( -0.000000000000000000, -0.000000000000000000, -1.000000000000000000 ) ) ;
#16266 = EDGE_CURVE ( 'NONE', #4656, #7706, #1793, .T. ) ;
#16267 = DIRECTION ( 'NONE',  ( 0.000000000000000000, -1.000000000000000000, 0.000000000000000000 ) ) ;
#16268 = DIRECTION ( 'NONE',  ( 1.000000000000000000, 0.000000000000000000, 0.000000000000000000 ) ) ;
#16269 = CARTESIAN_POINT ( 'NONE',  ( -2.935661446562617183, 9.035036904803758873, 2.659589141758143871 ) ) ;
#16270 = ORIENTED_EDGE ( 'NONE', *, *, #5164, .F. ) ;
#16271 = CARTESIAN_POINT ( 'NONE',  ( 0.000000000000000000, 0.000000000000000000, 53.00000000000000000 ) ) ;
#16272 = DIRECTION ( 'NONE',  ( -1.000000000000000000, -0.000000000000000000, -0.000000000000000000 ) ) ;
#16273 = CARTESIAN_POINT ( 'NONE',  ( 23.00000000000000000, -1.934484387511856252, -14.08058594723508072 ) ) ;
#16274 = ORIENTED_EDGE ( 'NONE', *, *, #11501, .T. ) ;
#16275 = ORIENTED_EDGE ( 'NONE', *, *, #20595, .F. ) ;
#16276 = DIRECTION ( 'NONE',  ( -1.000000000000000000, 0.000000000000000000, 0.000000000000000000 ) ) ;
#16277 = ORIENTED_EDGE ( 'NONE', *, *, #16470, .F. ) ;
#16278 = DIRECTION ( 'NONE',  ( 1.000000000000000000, 0.000000000000000000, 0.000000000000000000 ) ) ;
#16279 = DIRECTION ( 'NONE',  ( -0.5000000000000001110, -0.8660254037844384856, 0.000000000000000000 ) ) ;
#16280 = CARTESIAN_POINT ( 'NONE',  ( -9.500000000000000000, -6.482511860946779655E-13, 6.206742014460234103 ) ) ;
#16281 = ADVANCED_FACE ( 'NONE', ( #22283 ), #21922, .T. ) ;
#16282 = ADVANCED_FACE ( 'NONE', ( #10907 ), #12638, .T. ) ;
#16283 = CARTESIAN_POINT ( 'NONE',  ( 0.000000000000000000, 45.00000000000000000, 23.99999999999999645 ) ) ;
#16284 = DIRECTION ( 'NONE',  ( 0.000000000000000000, 1.000000000000000000, 0.000000000000000000 ) ) ;
#16285 = CIRCLE ( 'NONE', #15914, 4.171999999999999709 ) ;
#16286 = DIRECTION ( 'NONE',  ( -1.000000000000000000, 0.000000000000000000, 0.000000000000000000 ) ) ;
#16287 = FACE_OUTER_BOUND ( 'NONE', #5741, .T. ) ;
#16288 = VECTOR ( 'NONE', #17478, 1000.000000000000000 ) ;
#16289 = DIRECTION ( 'NONE',  ( 0.000000000000000000, -1.000000000000000000, 0.000000000000000000 ) ) ;
#16290 = CARTESIAN_POINT ( 'NONE',  ( -41.73082370883260950, 27.62204025492845716, -1.500000000000000000 ) ) ;
#16291 = DIRECTION ( 'NONE',  ( -1.000000000000000000, -0.000000000000000000, -0.000000000000000000 ) ) ;
#16292 = CARTESIAN_POINT ( 'NONE',  ( 7.022953521755574080, -5.102474405759714671, 10.43316557810918788 ) ) ;
#16293 = ORIENTED_EDGE ( 'NONE', *, *, #4251, .T. ) ;
#16294 = DIRECTION ( 'NONE',  ( 1.000000000000000000, 0.000000000000000000, 0.000000000000000000 ) ) ;
#16295 = DIRECTION ( 'NONE',  ( 0.000000000000000000, 0.000000000000000000, 1.000000000000000000 ) ) ;
#16296 = ORIENTED_EDGE ( 'NONE', *, *, #17575, .F. ) ;
#16297 = ORIENTED_EDGE ( 'NONE', *, *, #12223, .T. ) ;
#16298 = CARTESIAN_POINT ( 'NONE',  ( -8.133158128751217575, 4.897985262767988068, -12.01970669115188350 ) ) ;
#16299 = CARTESIAN_POINT ( 'NONE',  ( 6.809999908187194197E-13, -9.988891130263535700, -5.559589141758142894 ) ) ;
#16300 = PRESENTATION_LAYER_ASSIGNMENT (  '', '', ( #1889 ) ) ;
#16301 = DIRECTION ( 'NONE',  ( -1.000000000000000000, 0.000000000000000000, 0.000000000000000000 ) ) ;
#16302 = DIRECTION ( 'NONE',  ( -0.9913301211009810654, 0.1313947906041722236, -3.439367267033602767E-15 ) ) ;
#16303 = CYLINDRICAL_SURFACE ( 'NONE', #4517, 1.999999999999996669 ) ;
#16304 = DIRECTION ( 'NONE',  ( -0.000000000000000000, 0.000000000000000000, 1.000000000000000000 ) ) ;
#16305 = LINE ( 'NONE', #3615, #19606 ) ;
#16306 = EDGE_CURVE ( 'NONE', #22066, #7111, #22758, .T. ) ;
#16307 = CIRCLE ( 'NONE', #23731, 5.000000000000007994 ) ;
#16308 = EDGE_CURVE ( 'NONE', #6942, #1952, #84, .T. ) ;
#16309 = CARTESIAN_POINT ( 'NONE',  ( 60.32931906745326245, -4.999999999999999112, 0.000000000000000000 ) ) ;
#16310 = ORIENTED_EDGE ( 'NONE', *, *, #8076, .F. ) ;
#16311 = CARTESIAN_POINT ( 'NONE',  ( -30.68762588338046982, -45.64284848299540442, -3.000000000000000000 ) ) ;
#16312 = DIRECTION ( 'NONE',  ( 1.000000000000000000, 0.000000000000000000, 0.000000000000000000 ) ) ;
#16313 = CARTESIAN_POINT ( 'NONE',  ( 17.38971744193259994, 8.915620082851745565, -3.315798060087243648 ) ) ;
#16314 = DIRECTION ( 'NONE',  ( -1.000000000000000000, -0.000000000000000000, -0.000000000000000000 ) ) ;
#16315 = ORIENTED_EDGE ( 'NONE', *, *, #626, .T. ) ;
#16316 = DIRECTION ( 'NONE',  ( 1.000000000000000000, 0.000000000000000000, 0.000000000000000000 ) ) ;
#16317 = CARTESIAN_POINT ( 'NONE',  ( 9.500000000000209610, -3.086737114211962396, -9.106742014460232681 ) ) ;
#16318 = SURFACE_SIDE_STYLE ('',( #9112 ) ) ;
#16319 = ORIENTED_EDGE ( 'NONE', *, *, #17024, .T. ) ;
#16320 = ORIENTED_EDGE ( 'NONE', *, *, #6502, .F. ) ;
#16321 = CARTESIAN_POINT ( 'NONE',  ( -7.685661446562381371, 5.583959896777970222, 10.00674201446023481 ) ) ;
#16322 = CARTESIAN_POINT ( 'NONE',  ( 7.685661446561619314, 5.583959896779020049, 5.406742014460233392 ) ) ;
#16323 = LINE ( 'NONE', #12529, #20907 ) ;
#16324 = ORIENTED_EDGE ( 'NONE', *, *, #5021, .T. ) ;
#16325 = VERTEX_POINT ( 'NONE', #5336 ) ;
#16326 = DIRECTION ( 'NONE',  ( 0.000000000000000000, 0.000000000000000000, -1.000000000000000000 ) ) ;
#16327 = DIRECTION ( 'NONE',  ( -1.000000000000000000, 0.000000000000000000, 0.000000000000000000 ) ) ;
#16328 = DIRECTION ( 'NONE',  ( 0.000000000000000000, 0.000000000000000000, -1.000000000000000000 ) ) ;
#16329 = VECTOR ( 'NONE', #824, 1000.000000000000000 ) ;
#16330 = ADVANCED_FACE ( 'NONE', ( #20221 ), #10800, .T. ) ;
#16331 = CARTESIAN_POINT ( 'NONE',  ( -0.9830802669677229932, 45.00000000000000000, 0.000000000000000000 ) ) ;
#16332 = DIRECTION ( 'NONE',  ( 0.000000000000000000, -1.000000000000000000, 0.000000000000000000 ) ) ;
#16333 = VECTOR ( 'NONE', #17506, 1000.000000000000000 ) ;
#16334 = ADVANCED_FACE ( 'NONE', ( #22060 ), #4447, .F. ) ;
#16335 = DIRECTION ( 'NONE',  ( -0.000000000000000000, -0.000000000000000000, -1.000000000000000000 ) ) ;
#16336 = EDGE_CURVE ( 'NONE', #4197, #11455, #5220, .T. ) ;
#16337 = EDGE_LOOP ( 'NONE', ( #14683, #4486, #11488 ) ) ;
#16338 = CARTESIAN_POINT ( 'NONE',  ( -40.89823313241237912, 26.41789760203348081, -27.00000000000000000 ) ) ;
#16339 = SURFACE_STYLE_FILL_AREA ( #3299 ) ;
#16340 = CARTESIAN_POINT ( 'NONE',  ( -8.238183179803327150, 4.770819190637570983, -3.499164564451821224 ) ) ;
#16341 = DIRECTION ( 'NONE',  ( -1.000000000000000000, -1.224606353822377258E-16, -0.000000000000000000 ) ) ;
#16342 = DIRECTION ( 'NONE',  ( 0.000000000000000000, -1.000000000000000000, 0.000000000000000000 ) ) ;
#16343 = CIRCLE ( 'NONE', #12048, 5.000000000000007994 ) ;
#16344 = DIRECTION ( 'NONE',  ( 0.000000000000000000, 0.000000000000000000, -1.000000000000000000 ) ) ;
#16345 = ORIENTED_EDGE ( 'NONE', *, *, #1849, .T. ) ;
#16346 = CARTESIAN_POINT ( 'NONE',  ( 1.999999999999994449, -45.00000000000000000, 23.99999999999999645 ) ) ;
#16347 = VERTEX_POINT ( 'NONE', #691 ) ;
#16348 = AXIS2_PLACEMENT_3D ( 'NONE', #17335, #9743, #13560 ) ;
#16349 = CARTESIAN_POINT ( 'NONE',  ( 14.51962751333974389, -3.765689428759035895, 27.00000000000000000 ) ) ;
#16350 = ORIENTED_EDGE ( 'NONE', *, *, #10545, .T. ) ;
#16351 = DIRECTION ( 'NONE',  ( 1.000000000000000000, 0.000000000000000000, 0.000000000000000000 ) ) ;
#16352 = CARTESIAN_POINT ( 'NONE',  ( 40.77574956473004164, 27.49633847812775755, 12.00000000000000000 ) ) ;
#16353 = DIRECTION ( 'NONE',  ( -0.000000000000000000, -0.000000000000000000, 1.000000000000000000 ) ) ;
#16354 = DIRECTION ( 'NONE',  ( 0.5735764363510424957, 0.8191520442889943521, 0.000000000000000000 ) ) ;
#16355 = EDGE_CURVE ( 'NONE', #14736, #16231, #21192, .T. ) ;
#16356 = DIRECTION ( 'NONE',  ( 0.000000000000000000, -1.000000000000000000, 0.000000000000000000 ) ) ;
#16357 = CARTESIAN_POINT ( 'NONE',  ( 5.871322893124553133, -8.081182679343980269, -6.906742014460234280 ) ) ;
#16358 = ORIENTED_EDGE ( 'NONE', *, *, #2579, .T. ) ;
#16359 = CARTESIAN_POINT ( 'NONE',  ( -39.99999999999999289, 29.50000000000000000, 27.00000000000000000 ) ) ;
#16360 = CARTESIAN_POINT ( 'NONE',  ( -28.99999999999999645, 29.50000000000000000, -3.000000000000000000 ) ) ;
#16361 = EDGE_CURVE ( 'NONE', #12612, #15963, #16887, .T. ) ;
#16362 = DIRECTION ( 'NONE',  ( -1.000000000000000000, -0.000000000000000000, -0.000000000000000000 ) ) ;
#16363 = EDGE_CURVE ( 'NONE', #19575, #19379, #20034, .T. ) ;
#16364 = VERTEX_POINT ( 'NONE', #5920 ) ;
#16365 = CARTESIAN_POINT ( 'NONE',  ( 0.000000000000000000, -45.00000000000000000, 26.97499999999999432 ) ) ;
#16366 = DIRECTION ( 'NONE',  ( 0.000000000000000000, 0.000000000000000000, 1.000000000000000000 ) ) ;
#16367 = EDGE_LOOP ( 'NONE', ( #4412, #18840, #17492, #10674 ) ) ;
#16368 = DIRECTION ( 'NONE',  ( 0.000000000000000000, 0.000000000000000000, 1.000000000000000000 ) ) ;
#16369 = CARTESIAN_POINT ( 'NONE',  ( 35.99999999999999289, -51.00000000000000711, 0.5000000000000004441 ) ) ;
#16370 = CARTESIAN_POINT ( 'NONE',  ( 1.000000000000000222, 1.224646799147353454E-16, 4.000000000000000000 ) ) ;
#16371 = EDGE_LOOP ( 'NONE', ( #22132, #13536, #20643, #6649 ) ) ;
#16372 = CARTESIAN_POINT ( 'NONE',  ( 47.34180362313352930, -6.000000000000016875, 11.00000000000000000 ) ) ;
#16373 =( BOUNDED_CURVE ( )  B_SPLINE_CURVE ( 3, ( #14878, #23037, #6312, #5636 ),
 .UNSPECIFIED., .F., .T. ) 
 B_SPLINE_CURVE_WITH_KNOTS ( ( 4, 4 ),
 ( 0.000000000000000000, 1.570796326794896558 ),
 .UNSPECIFIED. ) 
 CURVE ( )  GEOMETRIC_REPRESENTATION_ITEM ( )  RATIONAL_B_SPLINE_CURVE ( ( 1.000000000000000000, 0.8047378541243649375, 0.8047378541243649375, 1.000000000000000000 ) ) 
 REPRESENTATION_ITEM ( '' )  );
#16374 = TOROIDAL_SURFACE ( 'NONE', #19515, 5.999999999999999112, 1.000000000000000000 ) ;
#16375 = EDGE_CURVE ( 'NONE', #11227, #6327, #18861, .T. ) ;
#16376 = ORIENTED_EDGE ( 'NONE', *, *, #7730, .T. ) ;
#16377 = EDGE_LOOP ( 'NONE', ( #8205, #23451, #11904, #12877, #16221 ) ) ;
#16378 = EDGE_CURVE ( 'NONE', #3826, #5746, #13395, .T. ) ;
#16379 = VERTEX_POINT ( 'NONE', #324 ) ;
#16380 = DIRECTION ( 'NONE',  ( -1.000000000000000000, -1.224606353822377258E-16, -0.000000000000000000 ) ) ;
#16381 = DIRECTION ( 'NONE',  ( -0.000000000000000000, -0.000000000000000000, 1.000000000000000000 ) ) ;
#16382 = ORIENTED_EDGE ( 'NONE', *, *, #22522, .T. ) ;
#16383 = ORIENTED_EDGE ( 'NONE', *, *, #22034, .T. ) ;
#16384 = DIRECTION ( 'NONE',  ( -1.000000000000000000, 0.000000000000000000, 0.000000000000000000 ) ) ;
#16385 = EDGE_CURVE ( 'NONE', #4863, #19008, #4050, .T. ) ;
#16386 = EDGE_CURVE ( 'NONE', #13623, #19012, #22768, .T. ) ;
#16387 = DIRECTION ( 'NONE',  ( -1.000000000000000000, 0.000000000000000000, 0.000000000000000000 ) ) ;
#16388 = VERTEX_POINT ( 'NONE', #19361 ) ;
#16389 = CARTESIAN_POINT ( 'NONE',  ( -20.64923905428956630, 37.45138642374539018, 11.00000000000000000 ) ) ;
#16390 = CARTESIAN_POINT ( 'NONE',  ( -7.685661446562381371, 5.583959896777970222, 6.006742014460233037 ) ) ;
#16391 = CARTESIAN_POINT ( 'NONE',  ( 0.1973939736642952303, 9.000000000000003553, 78.00000000000000000 ) ) ;
#16392 = VECTOR ( 'NONE', #6559, 1000.000000000000000 ) ;
#16393 = DIRECTION ( 'NONE',  ( 0.000000000000000000, 0.000000000000000000, -1.000000000000000000 ) ) ;
#16394 = CARTESIAN_POINT ( 'NONE',  ( 2.935661446562616295, -9.035036904803758873, 10.80674201446023197 ) ) ;
#16395 = AXIS2_PLACEMENT_3D ( 'NONE', #16908, #1563, #16420 ) ;
#16396 = CARTESIAN_POINT ( 'NONE',  ( -40.50000000000000000, -51.00000000000000711, 12.50000000000000000 ) ) ;
#16397 = CARTESIAN_POINT ( 'NONE',  ( -29.00000000000000000, -29.49999999999999645, 11.00000000000000000 ) ) ;
#16398 = CARTESIAN_POINT ( 'NONE',  ( 0.000000000000000000, 15.03999999999999915, -25.00000000000000000 ) ) ;
#16399 = DIRECTION ( 'NONE',  ( -0.000000000000000000, -0.000000000000000000, -1.000000000000000000 ) ) ;
#16400 = CARTESIAN_POINT ( 'NONE',  ( -8.680847955711200825, 2.820578480813073607, 11.53316557810918574 ) ) ;
#16401 = ORIENTED_EDGE ( 'NONE', *, *, #4596, .F. ) ;
#16402 = ADVANCED_FACE ( 'NONE', ( #5805 ), #2634, .F. ) ;
#16403 = SHAPE_DEFINITION_REPRESENTATION ( #16982, #21748 ) ;
#16404 = FACE_OUTER_BOUND ( 'NONE', #13708, .T. ) ;
#16405 = VECTOR ( 'NONE', #8537, 1000.000000000000000 ) ;
#16406 = ORIENTED_EDGE ( 'NONE', *, *, #1639, .F. ) ;
#16407 = EDGE_LOOP ( 'NONE', ( #17591, #1499, #12754, #16766 ) ) ;
#16408 = ADVANCED_FACE ( 'NONE', ( #20821 ), #13493, .T. ) ;
#16409 = CIRCLE ( 'NONE', #7880, 5.000000000000007994 ) ;
#16410 = DIRECTION ( 'NONE',  ( 0.000000000000000000, 0.8660254037844379305, -0.5000000000000013323 ) ) ;
#16411 = CARTESIAN_POINT ( 'NONE',  ( -2.935661446561384391, -9.035036904804158553, -3.459589141758144137 ) ) ;
#16412 = AXIS2_PLACEMENT_3D ( 'NONE', #6145, #21030, #18712 ) ;
#16413 = FACE_OUTER_BOUND ( 'NONE', #6472, .T. ) ;
#16414 = DIRECTION ( 'NONE',  ( -0.000000000000000000, 1.000000000000000000, -0.000000000000000000 ) ) ;
#16415 = DIRECTION ( 'NONE',  ( -1.000000000000000000, -0.000000000000000000, -0.000000000000000000 ) ) ;
#16416 = DIRECTION ( 'NONE',  ( -1.000000000000000000, -1.224606353822377258E-16, -0.000000000000000000 ) ) ;
#16417 = CARTESIAN_POINT ( 'NONE',  ( 0.000000000000000000, 0.000000000000000000, 12.50000000000000000 ) ) ;
#16418 = ORIENTED_EDGE ( 'NONE', *, *, #16755, .F. ) ;
#16419 = CARTESIAN_POINT ( 'NONE',  ( 0.000000000000000000, 0.000000000000000000, 103.9999999999999858 ) ) ;
#16420 = DIRECTION ( 'NONE',  ( 0.000000000000000000, -0.7557495743542638200, 0.6548607339452786613 ) ) ;
#16421 = DIRECTION ( 'NONE',  ( 0.000000000000000000, 0.000000000000000000, 1.000000000000000000 ) ) ;
#16422 = CARTESIAN_POINT ( 'NONE',  ( 17.57797814737054409, 9.461914562436920306, 0.9781177603712970514 ) ) ;
#16423 = CARTESIAN_POINT ( 'NONE',  ( 31.49999999999999289, 50.99999999999999289, 12.50000000000000000 ) ) ;
#16424 = ORIENTED_EDGE ( 'NONE', *, *, #22174, .T. ) ;
#16425 = DIRECTION ( 'NONE',  ( 0.000000000000000000, 0.000000000000000000, -1.000000000000000000 ) ) ;
#16426 = CARTESIAN_POINT ( 'NONE',  ( 9.500000000000209610, -3.086737114211962396, -11.10674201446023446 ) ) ;
#16427 = AXIS2_PLACEMENT_3D ( 'NONE', #11355, #20918, #6256 ) ;
#16428 = CARTESIAN_POINT ( 'NONE',  ( -39.99999999999999289, -29.50000000000001066, -27.00000000000000000 ) ) ;
#16429 = ORIENTED_EDGE ( 'NONE', *, *, #8347, .F. ) ;
#16430 = ORIENTED_EDGE ( 'NONE', *, *, #373, .F. ) ;
#16431 = CARTESIAN_POINT ( 'NONE',  ( 5.871322893124553133, -8.081182679343980269, 8.906742014460233392 ) ) ;
#16432 = CARTESIAN_POINT ( 'NONE',  ( -2.935661446562617183, 9.035036904803758873, 7.806742014460233747 ) ) ;
#16433 = ORIENTED_EDGE ( 'NONE', *, *, #15208, .T. ) ;
#16434 = ORIENTED_EDGE ( 'NONE', *, *, #8706, .F. ) ;
#16435 =( NAMED_UNIT ( * ) SI_UNIT ( $, .STERADIAN. ) SOLID_ANGLE_UNIT ( ) );
#16436 = LINE ( 'NONE', #23903, #15041 ) ;
#16437 = EDGE_CURVE ( 'NONE', #13710, #14422, #20943, .T. ) ;
#16438 = CARTESIAN_POINT ( 'NONE',  ( -2.935661446561384391, -9.035036904804158553, -4.606742014460233570 ) ) ;
#16439 = EDGE_CURVE ( 'NONE', #16829, #20146, #16894, .T. ) ;
#16440 = VECTOR ( 'NONE', #21707, 1000.000000000000000 ) ;
#16441 = LINE ( 'NONE', #3771, #8306 ) ;
#16442 = AXIS2_PLACEMENT_3D ( 'NONE', #11292, #2, #22098 ) ;
#16443 = LINE ( 'NONE', #1227, #1434 ) ;
#16444 = DIRECTION ( 'NONE',  ( -1.000000000000000000, -1.224606353822377258E-16, -0.000000000000000000 ) ) ;
#16445 = AXIS2_PLACEMENT_3D ( 'NONE', #16850, #22720, #18950 ) ;
#16446 = CIRCLE ( 'NONE', #19591, 50.00000000000000000 ) ;
#16447 = VECTOR ( 'NONE', #1770, 1000.000000000000000 ) ;
#16448 = ORIENTED_EDGE ( 'NONE', *, *, #5697, .F. ) ;
#16449 = AXIS2_PLACEMENT_3D ( 'NONE', #5770, #10981, #14897 ) ;
#16450 = EDGE_LOOP ( 'NONE', ( #15882, #8971, #4311, #17964, #1996, #2038, #20731, #7177, #11683, #11250, #12299, #11359, #17156, #18531, #17572 ) ) ;
#16451 = DIRECTION ( 'NONE',  ( 1.000000000000000000, 0.000000000000000000, 0.000000000000000000 ) ) ;
#16452 = PLANE ( 'NONE',  #11411 ) ;
#16453 = CYLINDRICAL_SURFACE ( 'NONE', #18031, 1.999999999999996669 ) ;
#16454 = DIRECTION ( 'NONE',  ( 1.000000000000000000, 0.000000000000000000, 0.000000000000000000 ) ) ;
#16455 = CARTESIAN_POINT ( 'NONE',  ( 6.250000000000000000, 10.82531754730548279, 2.500000000000000000 ) ) ;
#16456 = CARTESIAN_POINT ( 'NONE',  ( 85.63636363636365445, 4.172000000000015696, 0.000000000000000000 ) ) ;
#16457 = EDGE_LOOP ( 'NONE', ( #9870, #15790, #182, #5639 ) ) ;
#16458 = ADVANCED_FACE ( 'NONE', ( #9795 ), #17706, .T. ) ;
#16459 = DIRECTION ( 'NONE',  ( 1.000000000000000000, 0.000000000000000000, 0.000000000000000000 ) ) ;
#16460 = VERTEX_POINT ( 'NONE', #20686 ) ;
#16461 = CIRCLE ( 'NONE', #7113, 2.024999999999999911 ) ;
#16462 = DIRECTION ( 'NONE',  ( -1.000000000000000000, -1.224606353822377258E-16, -0.000000000000000000 ) ) ;
#16463 = CIRCLE ( 'NONE', #5955, 2.000000000000000000 ) ;
#16464 = CIRCLE ( 'NONE', #7878, 1.000000000000000888 ) ;
#16465 = VECTOR ( 'NONE', #17327, 1000.000000000000000 ) ;
#16466 = VECTOR ( 'NONE', #19786, 1000.000000000000000 ) ;
#16467 = ORIENTED_EDGE ( 'NONE', *, *, #8592, .T. ) ;
#16468 = DIRECTION ( 'NONE',  ( 0.000000000000000000, -0.7557495743542637090, 0.6548607339452788834 ) ) ;
#16469 = CIRCLE ( 'NONE', #11015, 0.4000000000000001887 ) ;
#16470 = EDGE_CURVE ( 'NONE', #10631, #14244, #178, .T. ) ;
#16471 = CARTESIAN_POINT ( 'NONE',  ( 20.85000000000000497, -16.67999999999999616, 14.50000000000000000 ) ) ;
#16472 = CARTESIAN_POINT ( 'NONE',  ( 1.500000000000001332, 0.000000000000000000, 0.000000000000000000 ) ) ;
#16473 = AXIS2_PLACEMENT_3D ( 'NONE', #4971, #19845, #4720 ) ;
#16474 = ADVANCED_FACE ( 'NONE', ( #22897 ), #3969, .F. ) ;
#16475 = CYLINDRICAL_SURFACE ( 'NONE', #11479, 6.050000000006051870 ) ;
#16476 = EDGE_CURVE ( 'NONE', #2444, #21069, #6410, .T. ) ;
#16477 = EDGE_CURVE ( 'NONE', #9290, #14927, #2510, .T. ) ;
#16478 = AXIS2_PLACEMENT_3D ( 'NONE', #7549, #13054, #7325 ) ;
#16479 = ORIENTED_EDGE ( 'NONE', *, *, #1132, .T. ) ;
#16480 = DIRECTION ( 'NONE',  ( 1.000000000000000000, 0.000000000000000000, 0.000000000000000000 ) ) ;
#16481 = DIRECTION ( 'NONE',  ( -1.000000000000000000, 0.000000000000000000, 0.000000000000000000 ) ) ;
#16482 = CARTESIAN_POINT ( 'NONE',  ( -5.871322893124554021, 8.081182679343978492, -8.759589141758141295 ) ) ;
#16483 = VERTEX_POINT ( 'NONE', #15804 ) ;
#16484 = ORIENTED_EDGE ( 'NONE', *, *, #7448, .T. ) ;
#16485 = CARTESIAN_POINT ( 'NONE',  ( -40.66734255040738333, 26.56420859267091927, -3.000000000000000000 ) ) ;
#16486 = DIRECTION ( 'NONE',  ( 1.000000000000000000, 0.000000000000000000, 0.000000000000000000 ) ) ;
#16487 = CIRCLE ( 'NONE', #9829, 5.024999999999998579 ) ;
#16488 = AXIS2_PLACEMENT_3D ( 'NONE', #23665, #18387, #8976 ) ;
#16489 = DIRECTION ( 'NONE',  ( -1.000000000000000000, 1.387778780781444492E-15, 0.000000000000000000 ) ) ;
#16490 = AXIS2_PLACEMENT_3D ( 'NONE', #15030, #7584, #12963 ) ;
#16491 = DIRECTION ( 'NONE',  ( 0.000000000000000000, 0.000000000000000000, 1.000000000000000000 ) ) ;
#16492 = AXIS2_PLACEMENT_3D ( 'NONE', #16681, #336, #14833 ) ;
#16493 = ORIENTED_EDGE ( 'NONE', *, *, #4525, .F. ) ;
#16494 = DIRECTION ( 'NONE',  ( -0.9913301211009810654, 0.1313947906041722236, 0.000000000000000000 ) ) ;
#16495 = DIRECTION ( 'NONE',  ( 1.000000000000000000, 0.000000000000000000, 0.000000000000000000 ) ) ;
#16496 = ADVANCED_FACE ( 'NONE', ( #17502 ), #23270, .F. ) ;
#16497 = CARTESIAN_POINT ( 'NONE',  ( 80.69295543108962931, 7.420530141404717394E-15, 0.000000000000000000 ) ) ;
#16498 = ORIENTED_EDGE ( 'NONE', *, *, #1288, .F. ) ;
#16499 = DIRECTION ( 'NONE',  ( -1.000000000000000000, 0.000000000000000000, 0.000000000000000000 ) ) ;
#16500 = DIRECTION ( 'NONE',  ( -1.000000000000000000, -1.224606353822377258E-16, -0.000000000000000000 ) ) ;
#16501 = DIRECTION ( 'NONE',  ( -1.000000000000000000, 0.000000000000000000, 0.000000000000000000 ) ) ;
#16502 = CARTESIAN_POINT ( 'NONE',  ( -41.99999999999999289, -25.93535998569255341, -27.00000000000000000 ) ) ;
#16503 = ADVANCED_FACE ( 'NONE', ( #21668 ), #3004, .T. ) ;
#16504 = AXIS2_PLACEMENT_3D ( 'NONE', #11184, #6, #7410 ) ;
#16505 = VERTEX_POINT ( 'NONE', #14088 ) ;
#16506 = EDGE_CURVE ( 'NONE', #1409, #15508, #1354, .T. ) ;
#16507 = ORIENTED_EDGE ( 'NONE', *, *, #18701, .F. ) ;
#16508 = EDGE_CURVE ( 'NONE', #14186, #9926, #21209, .T. ) ;
#16509 = AXIS2_PLACEMENT_3D ( 'NONE', #17087, #22591, #21006 ) ;
#16510 = AXIS2_PLACEMENT_3D ( 'NONE', #13119, #433, #7614 ) ;
#16512 = ORIENTED_EDGE ( 'NONE', *, *, #18657, .T. ) ;
#16511 = AXIS2_PLACEMENT_3D ( 'NONE', #5076, #18006, #12622 ) ;
#16513 = DIRECTION ( 'NONE',  ( -0.7071067811865474617, 0.000000000000000000, -0.7071067811865474617 ) ) ;
#16514 = AXIS2_PLACEMENT_3D ( 'NONE', #13893, #23654, #10194 ) ;
#16515 = CARTESIAN_POINT ( 'NONE',  ( 0.000000000000000000, -15.03999999999999915, -27.00000000000000000 ) ) ;
#16516 = ORIENTED_EDGE ( 'NONE', *, *, #22772, .F. ) ;
#16517 = CIRCLE ( 'NONE', #12630, 8.000000000000000000 ) ;
#16518 = ORIENTED_EDGE ( 'NONE', *, *, #16477, .F. ) ;
#16519 = DIRECTION ( 'NONE',  ( 0.000000000000000000, -1.000000000000000000, 0.000000000000000000 ) ) ;
#16520 = VERTEX_POINT ( 'NONE', #19944 ) ;
#16521 = CARTESIAN_POINT ( 'NONE',  ( -9.383344417114237501, 0.2560680661589281315, 12.11665558288575184 ) ) ;
#16522 = DIRECTION ( 'NONE',  ( -1.000000000000000000, 0.000000000000000000, 0.000000000000000000 ) ) ;
#16523 = DIRECTION ( 'NONE',  ( -0.000000000000000000, -0.000000000000000000, -1.000000000000000000 ) ) ;
#16524 = DIRECTION ( 'NONE',  ( 1.000000000000000000, -4.625929269271486900E-15, 0.000000000000000000 ) ) ;
#16525 = AXIS2_PLACEMENT_3D ( 'NONE', #18388, #8977, #1682 ) ;
#16526 = CARTESIAN_POINT ( 'NONE',  ( 65.27272727272728048, 7.491529369508391930E-15, 0.000000000000000000 ) ) ;
#16527 = DIRECTION ( 'NONE',  ( 0.000000000000000000, 0.000000000000000000, 1.000000000000000000 ) ) ;
#16528 = DIRECTION ( 'NONE',  ( -1.000000000000000000, 0.000000000000000000, 0.000000000000000000 ) ) ;
#16529 = ORIENTED_EDGE ( 'NONE', *, *, #8354, .F. ) ;
#16530 = VECTOR ( 'NONE', #18219, 1000.000000000000000 ) ;
#16531 = ORIENTED_EDGE ( 'NONE', *, *, #23461, .F. ) ;
#16532 = CARTESIAN_POINT ( 'NONE',  ( 5.365059087798938364, 7.384370330707087149, 8.933165578109186100 ) ) ;
#16533 = ORIENTED_EDGE ( 'NONE', *, *, #21075, .T. ) ;
#16534 = AXIS2_PLACEMENT_3D ( 'NONE', #2146, #18994, #14717 ) ;
#16535 = EDGE_CURVE ( 'NONE', #9670, #5201, #11441, .T. ) ;
#16536 = APPLICATION_PROTOCOL_DEFINITION ( 'draft international standard', 'automotive_design', 1998, #21014 ) ;
#16537 = CYLINDRICAL_SURFACE ( 'NONE', #15920, 5.000000000000000888 ) ;
#16538 = VERTEX_POINT ( 'NONE', #10047 ) ;
#16539 = ORIENTED_EDGE ( 'NONE', *, *, #16699, .T. ) ;
#16540 = PLANE ( 'NONE',  #16553 ) ;
#16541 = CARTESIAN_POINT ( 'NONE',  ( 7.022953521755574080, -5.102474405759714671, -12.43316557810918788 ) ) ;
#16542 = AXIS2_PLACEMENT_3D ( 'NONE', #16780, #9449, #15309 ) ;
#16543 = CARTESIAN_POINT ( 'NONE',  ( 9.090423977855502713, 6.191897047423500831E-13, 12.34637735993366725 ) ) ;
#16544 = DIRECTION ( 'NONE',  ( -0.4999999999999998890, -0.8660254037844385966, 0.000000000000000000 ) ) ;
#16545 = DIRECTION ( 'NONE',  ( 1.000000000000000000, 0.000000000000000000, -0.000000000000000000 ) ) ;
#16546 = DIRECTION ( 'NONE',  ( 0.1313947906041722513, -0.9913301211009810654, 0.000000000000000000 ) ) ;
#16547 = CYLINDRICAL_SURFACE ( 'NONE', #11369, 9.500000000000000000 ) ;
#16548 = ORIENTED_EDGE ( 'NONE', *, *, #3888, .F. ) ;
#16549 = CIRCLE ( 'NONE', #13043, 5.000000000000000888 ) ;
#16550 = EDGE_CURVE ( 'NONE', #18498, #3705, #10303, .T. ) ;
#16551 = CARTESIAN_POINT ( 'NONE',  ( 0.2999999999999999334, 1.766666099057062414E-15, -14.42592346043842433 ) ) ;
#16552 = CARTESIAN_POINT ( 'NONE',  ( 0.000000000000000000, 45.00000000000000000, -26.97499999999999432 ) ) ;
#16553 = AXIS2_PLACEMENT_3D ( 'NONE', #21920, #16410, #5557 ) ;
#16554 = CIRCLE ( 'NONE', #9153, 6.050000000006050982 ) ;
#16555 = DIRECTION ( 'NONE',  ( 0.000000000000000000, 0.000000000000000000, -1.000000000000000000 ) ) ;
#16556 = EDGE_CURVE ( 'NONE', #21563, #17766, #14953, .T. ) ;
#16557 = CARTESIAN_POINT ( 'NONE',  ( 89.12522638709219791, 7.562528597612068045E-15, 0.000000000000000000 ) ) ;
#16558 = CARTESIAN_POINT ( 'NONE',  ( -7.685661446561619314, -5.583959896779019161, -10.40674201446023339 ) ) ;
#16559 = SURFACE_STYLE_USAGE ( .BOTH. , #16318 ) ;
#16560 = ORIENTED_EDGE ( 'NONE', *, *, #18850, .T. ) ;
#16561 = EDGE_CURVE ( 'NONE', #21442, #13963, #14821, .T. ) ;
#16562 = ORIENTED_EDGE ( 'NONE', *, *, #6050, .F. ) ;
#16563 = CARTESIAN_POINT ( 'NONE',  ( -2.935661446562617183, 9.035036904803758873, 7.806742014460233747 ) ) ;
#16564 = ORIENTED_EDGE ( 'NONE', *, *, #16916, .T. ) ;
#16565 = VERTEX_POINT ( 'NONE', #5423 ) ;
#16566 = CIRCLE ( 'NONE', #20916, 5.000000000000007994 ) ;
#16567 = DIRECTION ( 'NONE',  ( -0.000000000000000000, 0.000000000000000000, -1.000000000000000000 ) ) ;
#16568 = VECTOR ( 'NONE', #9623, 1000.000000000000000 ) ;
#16569 = FACE_OUTER_BOUND ( 'NONE', #10285, .T. ) ;
#16570 = DIRECTION ( 'NONE',  ( 0.000000000000000000, 0.000000000000000000, 1.000000000000000000 ) ) ;
#16571 = DIRECTION ( 'NONE',  ( -1.000000000000000000, 0.000000000000000000, 0.000000000000000000 ) ) ;
#16572 = VECTOR ( 'NONE', #986, 1000.000000000000000 ) ;
#16573 = VECTOR ( 'NONE', #14754, 1000.000000000000000 ) ;
#16574 = FACE_OUTER_BOUND ( 'NONE', #3305, .T. ) ;
#16575 = DIRECTION ( 'NONE',  ( 1.000000000000000000, 0.000000000000000000, -0.000000000000000000 ) ) ;
#16576 = DIRECTION ( 'NONE',  ( -0.000000000000000000, -0.000000000000000000, -1.000000000000000000 ) ) ;
#16577 = ORIENTED_EDGE ( 'NONE', *, *, #12283, .T. ) ;
#16578 = CARTESIAN_POINT ( 'NONE',  ( 75.45454545454545325, 4.172000000000015696, 0.000000000000000000 ) ) ;
#16579 = AXIS2_PLACEMENT_3D ( 'NONE', #6198, #10195, #19628 ) ;
#16580 = DIRECTION ( 'NONE',  ( -1.000000000000000000, -0.000000000000000000, -0.000000000000000000 ) ) ;
#16581 = CARTESIAN_POINT ( 'NONE',  ( 9.376681730866099684, -1.188761456322485532, -12.06692573382535016 ) ) ;
#16582 = DIRECTION ( 'NONE',  ( 0.000000000000000000, 0.000000000000000000, 1.000000000000000000 ) ) ;
#16583 = AXIS2_PLACEMENT_3D ( 'NONE', #20245, #14262, #5359 ) ;
#16584 = CONICAL_SURFACE ( 'NONE', #14653, 4.172000000000008590, 0.9599310885968742602 ) ;
#16585 = DIRECTION ( 'NONE',  ( -1.000000000000000000, -1.224606353822377258E-16, -0.000000000000000000 ) ) ;
#16586 = EDGE_CURVE ( 'NONE', #9726, #6008, #23575, .T. ) ;
#16587 = EDGE_CURVE ( 'NONE', #23300, #11051, #4071, .T. ) ;
#16588 = CARTESIAN_POINT ( 'NONE',  ( -2.682529543899159208, -8.255977015246598327, -10.03316557810918930 ) ) ;
#16589 = AXIS2_PLACEMENT_3D ( 'NONE', #13365, #4110, #15300 ) ;
#16590 = CARTESIAN_POINT ( 'NONE',  ( -14.79187224938325507, 2.570168443617186771, 9.168425918763430715 ) ) ;
#16591 = CIRCLE ( 'NONE', #13873, 8.000000000000000000 ) ;
#16592 = ORIENTED_EDGE ( 'NONE', *, *, #11588, .T. ) ;
#16593 = DIRECTION ( 'NONE',  ( 0.000000000000000000, -0.000000000000000000, 1.000000000000000000 ) ) ;
#16594 = EDGE_LOOP ( 'NONE', ( #9240, #15022, #3728, #393 ) ) ;
#16595 = CARTESIAN_POINT ( 'NONE',  ( 2.935661446562616295, -9.035036904803758873, -9.659589141758143427 ) ) ;
#16596 = ORIENTED_EDGE ( 'NONE', *, *, #21733, .F. ) ;
#16597 = FACE_BOUND ( 'NONE', #2410, .T. ) ;
#16598 = DIRECTION ( 'NONE',  ( 0.000000000000000000, 0.000000000000000000, 1.000000000000000000 ) ) ;
#16599 = DIRECTION ( 'NONE',  ( -0.000000000000000000, -0.000000000000000000, -1.000000000000000000 ) ) ;
#16600 = VECTOR ( 'NONE', #3493, 1000.000000000000000 ) ;
#16601 = AXIS2_PLACEMENT_3D ( 'NONE', #3130, #18016, #3026 ) ;
#16602 = AXIS2_PLACEMENT_3D ( 'NONE', #16271, #12110, #23622 ) ;
#16603 = CARTESIAN_POINT ( 'NONE',  ( 5.000000000000000000, -4.685197434473820088, 9.540979117872439019E-15 ) ) ;
#16604 = CIRCLE ( 'NONE', #4156, 8.000000000000000000 ) ;
#16605 = TOROIDAL_SURFACE ( 'NONE', #22863, 10.49999999999999822, 1.000000000000000000 ) ;
#16606 = ADVANCED_FACE ( 'NONE', ( #22255 ), #4466, .T. ) ;
#16607 = CARTESIAN_POINT ( 'NONE',  ( -7.685661446562381371, 5.583959896777970222, -4.859589141758143604 ) ) ;
#16608 = VERTEX_POINT ( 'NONE', #11717 ) ;
#16609 = ORIENTED_EDGE ( 'NONE', *, *, #2189, .T. ) ;
#16610 = DIRECTION ( 'NONE',  ( 0.000000000000000000, 0.7557495743542551603, 0.6548607339452887643 ) ) ;
#16611 = CARTESIAN_POINT ( 'NONE',  ( 0.000000000000000000, -6.393861490227802591, -9.782270569456514409 ) ) ;
#16612 = DIRECTION ( 'NONE',  ( -1.000000000000000000, 0.000000000000000000, 0.000000000000000000 ) ) ;
#16613 = EDGE_CURVE ( 'NONE', #1596, #9356, #20434, .T. ) ;
#16614 = EDGE_CURVE ( 'NONE', #5101, #21243, #4972, .T. ) ;
#16615 = LINE ( 'NONE', #11462, #15122 ) ;
#16616 = EDGE_CURVE ( 'NONE', #6136, #11467, #7544, .T. ) ;
#16617 = AXIS2_PLACEMENT_3D ( 'NONE', #8059, #9889, #17465 ) ;
#16618 = CYLINDRICAL_SURFACE ( 'NONE', #23494, 5.099999999999996980 ) ;
#16619 = CARTESIAN_POINT ( 'NONE',  ( 43.99999999999999289, 50.99999999999999289, 0.5000000000000000000 ) ) ;
#16620 = EDGE_CURVE ( 'NONE', #1880, #22436, #9603, .T. ) ;
#16621 = VECTOR ( 'NONE', #13947, 1000.000000000000000 ) ;
#16622 = DIRECTION ( 'NONE',  ( -0.000000000000000000, -0.000000000000000000, -1.000000000000000000 ) ) ;
#16623 = ORIENTED_EDGE ( 'NONE', *, *, #19855, .F. ) ;
#16624 = DIRECTION ( 'NONE',  ( -0.7071067811865660024, 0.000000000000000000, -0.7071067811865291430 ) ) ;
#16625 = DIRECTION ( 'NONE',  ( -0.000000000000000000, 0.000000000000000000, -1.000000000000000000 ) ) ;
#16626 = LINE ( 'NONE', #22245, #4548 ) ;
#16627 = VECTOR ( 'NONE', #11940, 1000.000000000000000 ) ;
#16628 = CARTESIAN_POINT ( 'NONE',  ( -2.682529543900285862, 8.255977015246234174, 3.233165578109188587 ) ) ;
#16629 = VERTEX_POINT ( 'NONE', #4443 ) ;
#16630 = ORIENTED_EDGE ( 'NONE', *, *, #15331, .F. ) ;
#16631 = ORIENTED_EDGE ( 'NONE', *, *, #984, .T. ) ;
#16632 = AXIS2_PLACEMENT_3D ( 'NONE', #10534, #16276, #17996 ) ;
#16633 = ITEM_DEFINED_TRANSFORMATION ( 'NONE', 'NONE', #267,  #8005 ) ;
#16634 = ORIENTED_EDGE ( 'NONE', *, *, #23956, .T. ) ;
#16635 = DIRECTION ( 'NONE',  ( 0.8660254037844385966, -0.5000000000000003331, 0.000000000000000000 ) ) ;
#16636 = VECTOR ( 'NONE', #20605, 1000.000000000000000 ) ;
#16637 = EDGE_CURVE ( 'NONE', #12561, #18856, #9896, .T. ) ;
#16638 = CARTESIAN_POINT ( 'NONE',  ( 72.54545454545454675, 7.491529369508391930E-15, 0.000000000000000000 ) ) ;
#16639 = ORIENTED_EDGE ( 'NONE', *, *, #9839, .T. ) ;
#16640 = VERTEX_POINT ( 'NONE', #2835 ) ;
#16641 = DIRECTION ( 'NONE',  ( -0.8757121056631633760, -0.4828336235133056653, 0.000000000000000000 ) ) ;
#16642 = DIRECTION ( 'NONE',  ( -1.000000000000000000, 0.000000000000000000, 0.000000000000000000 ) ) ;
#16643 = ORIENTED_EDGE ( 'NONE', *, *, #23438, .F. ) ;
#16644 = FACE_OUTER_BOUND ( 'NONE', #8988, .T. ) ;
#16645 = DIRECTION ( 'NONE',  ( -0.7071067811865331398, 0.000000000000000000, 0.7071067811865620056 ) ) ;
#16646 = EDGE_CURVE ( 'NONE', #578, #7419, #11059, .T. ) ;
#16647 = EDGE_CURVE ( 'NONE', #18868, #23464, #10271, .T. ) ;
#16648 = DIRECTION ( 'NONE',  ( -1.000000000000000000, 0.000000000000000000, 0.000000000000000000 ) ) ;
#16649 = DIRECTION ( 'NONE',  ( 1.000000000000000000, -6.750155989720951766E-14, 0.000000000000000000 ) ) ;
#16650 = DIRECTION ( 'NONE',  ( -1.000000000000000000, -0.000000000000000000, 0.000000000000000000 ) ) ;
#16651 = DIRECTION ( 'NONE',  ( 0.000000000000000000, -1.000000000000000000, 0.000000000000000000 ) ) ;
#16652 = DIRECTION ( 'NONE',  ( 1.000000000000000000, 0.000000000000000000, 0.000000000000000000 ) ) ;
#16653 = CARTESIAN_POINT ( 'NONE',  ( 87.09090909090909349, 7.491529369508391930E-15, 0.000000000000000000 ) ) ;
#16654 = CARTESIAN_POINT ( 'NONE',  ( -14.99999999999999822, 6.045577542124163753E-21, -9.499999999999994671 ) ) ;
#16655 = ORIENTED_EDGE ( 'NONE', *, *, #8221, .F. ) ;
#16656 = VERTEX_POINT ( 'NONE', #8451 ) ;
#16657 = DIRECTION ( 'NONE',  ( -0.000000000000000000, -0.000000000000000000, -1.000000000000000000 ) ) ;
#16658 = ORIENTED_EDGE ( 'NONE', *, *, #7102, .T. ) ;
#16659 = SHAPE_DEFINITION_REPRESENTATION ( #7621, #19247 ) ;
#16660 = ORIENTED_EDGE ( 'NONE', *, *, #1932, .F. ) ;
#16661 = VERTEX_POINT ( 'NONE', #15899 ) ;
#16662 = PRODUCT_DEFINITION_SHAPE ( 'NONE', 'NONE',  #24118 ) ;
#16663 = DIRECTION ( 'NONE',  ( -0.000000000000000000, -0.000000000000000000, 1.000000000000000000 ) ) ;
#16664 = CARTESIAN_POINT ( 'NONE',  ( 2.682529543900284974, -8.255977015246234174, -10.23316557810918859 ) ) ;
#16665 = VERTEX_POINT ( 'NONE', #6628 ) ;
#16666 = CARTESIAN_POINT ( 'NONE',  ( 89.12522638709219791, 7.562528597612068045E-15, 0.000000000000000000 ) ) ;
#16667 = DIRECTION ( 'NONE',  ( -1.000000000000000000, 0.000000000000000000, 0.000000000000000000 ) ) ;
#16668 = DIRECTION ( 'NONE',  ( 1.000000000000000000, 0.000000000000000000, 0.000000000000000000 ) ) ;
#16669 = VECTOR ( 'NONE', #22065, 1000.000000000000000 ) ;
#16670 = FACE_OUTER_BOUND ( 'NONE', #10863, .T. ) ;
#16671 = ORIENTED_EDGE ( 'NONE', *, *, #13640, .T. ) ;
#16672 = CARTESIAN_POINT ( 'NONE',  ( 0.000000000000000000, 45.00000000000000000, 26.97499999999999432 ) ) ;
#16673 = ORIENTED_EDGE ( 'NONE', *, *, #22323, .T. ) ;
#16674 = EDGE_LOOP ( 'NONE', ( #22880, #22396, #23129, #12530 ) ) ;
#16675 = CARTESIAN_POINT ( 'NONE',  ( -0.9830802669677229932, 45.00000000000000000, 0.000000000000000000 ) ) ;
#16676 = EDGE_CURVE ( 'NONE', #18123, #22195, #23466, .T. ) ;
#16677 = CARTESIAN_POINT ( 'NONE',  ( -27.70933665152131198, 40.41277845351217479, 12.00000000000000000 ) ) ;
#16678 = DIRECTION ( 'NONE',  ( 0.000000000000000000, -1.000000000000000000, 0.000000000000000000 ) ) ;
#16679 = EDGE_CURVE ( 'NONE', #4095, #22047, #20048, .T. ) ;
#16680 = CARTESIAN_POINT ( 'NONE',  ( -28.73477696352898292, -42.73830357953205805, -1.500000000000000000 ) ) ;
#16681 = CARTESIAN_POINT ( 'NONE',  ( 5.000000000000000000, 4.685197434473818312, -1.301042606982605321E-15 ) ) ;
#16682 = CARTESIAN_POINT ( 'NONE',  ( 2.935661446561383503, 9.035036904804158553, -9.606742014460232681 ) ) ;
#16683 = CARTESIAN_POINT ( 'NONE',  ( -31.10231664966676846, -45.36128193761570770, 11.00000000000000000 ) ) ;
#16684 = ORIENTED_EDGE ( 'NONE', *, *, #11860, .T. ) ;
#16685 = EDGE_LOOP ( 'NONE', ( #4314, #11025, #1084, #14303, #2034 ) ) ;
#16686 = CARTESIAN_POINT ( 'NONE',  ( 9.500000000000000000, 6.470877716354879437E-13, 9.206742014460234103 ) ) ;
#16687 = ORIENTED_EDGE ( 'NONE', *, *, #11929, .T. ) ;
#16688 = AXIS2_PLACEMENT_3D ( 'NONE', #3745, #13496, #87 ) ;
#16689 = EDGE_LOOP ( 'NONE', ( #2558, #22643, #1522, #10929 ) ) ;
#16690 = CONICAL_SURFACE ( 'NONE', #10799, 2.024999999999999911, 0.7853981633974743692 ) ;
#16691 = AXIS2_PLACEMENT_3D ( 'NONE', #7222, #18221, #16612 ) ;
#16692 = ORIENTED_EDGE ( 'NONE', *, *, #12702, .T. ) ;
#16693 = CARTESIAN_POINT ( 'NONE',  ( -9.500000000000000000, -6.482511860946779655E-13, 9.059589141758143782 ) ) ;
#16694 = EDGE_CURVE ( 'NONE', #3225, #19080, #10859, .T. ) ;
#16695 = DIRECTION ( 'NONE',  ( -1.000000000000000000, -0.000000000000000000, 0.000000000000000000 ) ) ;
#16696 = DIRECTION ( 'NONE',  ( -1.000000000000000000, -0.000000000000000000, -0.000000000000000000 ) ) ;
#16697 = ADVANCED_FACE ( 'NONE', ( #1392 ), #13410, .F. ) ;
#16698 = CLOSED_SHELL ( 'NONE', ( #15054, #7949, #7563, #1202, #9394, #13711, #1438, #5766, #7397, #5166 ) ) ;
#16699 = EDGE_CURVE ( 'NONE', #23971, #9249, #2908, .T. ) ;
#16700 = LINE ( 'NONE', #4, #13848 ) ;
#16701 = CARTESIAN_POINT ( 'NONE',  ( 6.250000000000000000, 10.82531754730548279, 2.500000000000000000 ) ) ;
#16702 = CARTESIAN_POINT ( 'NONE',  ( -29.00000000000000000, -29.49999999999999645, 12.00000000000000000 ) ) ;
#16703 = CYLINDRICAL_SURFACE ( 'NONE', #118, 20.85000000000000142 ) ;
#16704 = DIRECTION ( 'NONE',  ( -1.000000000000000000, 0.000000000000000000, 0.000000000000000000 ) ) ;
#16705 = DIRECTION ( 'NONE',  ( -0.000000000000000000, -0.000000000000000000, -1.000000000000000000 ) ) ;
#16706 = VERTEX_POINT ( 'NONE', #20389 ) ;
#16707 = CARTESIAN_POINT ( 'NONE',  ( 0.000000000000000000, 0.000000000000000000, 15.50000000000000000 ) ) ;
#16708 = ORIENTED_EDGE ( 'NONE', *, *, #21568, .T. ) ;
#16709 = DIRECTION ( 'NONE',  ( 1.000000000000000000, 0.000000000000000000, 0.000000000000000000 ) ) ;
#16710 = CIRCLE ( 'NONE', #21019, 9.500000000000000000 ) ;
#16711 = ORIENTED_EDGE ( 'NONE', *, *, #10968, .T. ) ;
#16712 = FACE_OUTER_BOUND ( 'NONE', #20035, .T. ) ;
#16713 = DIRECTION ( 'NONE',  ( 0.5735764363510424957, 0.8191520442889943521, 0.000000000000000000 ) ) ;
#16714 = DIRECTION ( 'NONE',  ( -0.000000000000000000, -0.000000000000000000, -1.000000000000000000 ) ) ;
#16715 = ADVANCED_FACE ( 'NONE', ( #3195 ), #16909, .T. ) ;
#16716 = DIRECTION ( 'NONE',  ( 1.000000000000000000, 0.000000000000000000, 0.000000000000000000 ) ) ;
#16717 = CARTESIAN_POINT ( 'NONE',  ( 6.809999908187194197E-13, -9.988891130263535700, -5.559589141758142894 ) ) ;
#16718 = EDGE_LOOP ( 'NONE', ( #20322, #5756, #7826, #11120 ) ) ;
#16719 = EDGE_LOOP ( 'NONE', ( #13397, #10978 ) ) ;
#16720 = DIRECTION ( 'NONE',  ( 0.000000000000000000, 0.000000000000000000, 1.000000000000000000 ) ) ;
#16721 = ORIENTED_EDGE ( 'NONE', *, *, #20481, .T. ) ;
#16722 = CARTESIAN_POINT ( 'NONE',  ( 2.570122167802765922, 1.191082103573950341E-15, -9.725923461386811297 ) ) ;
#16723 = AXIS2_PLACEMENT_3D ( 'NONE', #8593, #14328, #12617 ) ;
#16724 = ORIENTED_EDGE ( 'NONE', *, *, #18738, .F. ) ;
#16725 = CARTESIAN_POINT ( 'NONE',  ( 43.99999999999999289, 50.99999999999999289, 0.5000000000000000000 ) ) ;
#16726 = DIRECTION ( 'NONE',  ( -1.000000000000000000, -0.000000000000000000, -0.000000000000000000 ) ) ;
#16727 = FACE_OUTER_BOUND ( 'NONE', #7603, .T. ) ;
#16728 = VERTEX_POINT ( 'NONE', #9036 ) ;
#16729 = CARTESIAN_POINT ( 'NONE',  ( 0.2999999999999999889, 0.000000000000000000, 10.02592346138681023 ) ) ;
#16730 = CARTESIAN_POINT ( 'NONE',  ( 60.90909090909091361, 7.491529369508391930E-15, 0.000000000000000000 ) ) ;
#16731 = DIRECTION ( 'NONE',  ( 0.7089874389501501506, -0.7052211081716905916, 0.000000000000000000 ) ) ;
#16732 = CARTESIAN_POINT ( 'NONE',  ( 82.14750088563508257, -9.244463733058732095E-30, 5.000000000000007994 ) ) ;
#16733 = CARTESIAN_POINT ( 'NONE',  ( 7.022953521755574080, -5.102474405759714671, 6.433165578109188765 ) ) ;
#16734 = ORIENTED_EDGE ( 'NONE', *, *, #7702, .T. ) ;
#16735 = ORIENTED_EDGE ( 'NONE', *, *, #21250, .T. ) ;
#16736 = ORIENTED_EDGE ( 'NONE', *, *, #9348, .T. ) ;
#16737 = AXIS2_PLACEMENT_3D ( 'NONE', #9256, #10948, #18199 ) ;
#16738 = EDGE_CURVE ( 'NONE', #11511, #14734, #14526, .T. ) ;
#16739 = ORIENTED_EDGE ( 'NONE', *, *, #23780, .T. ) ;
#16740 = DIRECTION ( 'NONE',  ( -1.000000000000000000, -1.224606353822377258E-16, -0.000000000000000000 ) ) ;
#16741 = EDGE_CURVE ( 'NONE', #4173, #20705, #1737, .T. ) ;
#16742 = DIRECTION ( 'NONE',  ( -1.000000000000000000, 0.000000000000000000, 0.000000000000000000 ) ) ;
#16743 = VERTEX_POINT ( 'NONE', #16359 ) ;
#16744 = DIRECTION ( 'NONE',  ( 0.000000000000000000, 0.000000000000000000, 1.000000000000000000 ) ) ;
#16745 = EDGE_LOOP ( 'NONE', ( #2409, #12009, #162, #7840, #9620, #2482 ) ) ;
#16746 = CARTESIAN_POINT ( 'NONE',  ( 58.57977184163763695, 7.562528597612068045E-15, 0.000000000000000000 ) ) ;
#16747 = CARTESIAN_POINT ( 'NONE',  ( 3.890962118697714531E-15, 15.50000000000000000, 12.50000000000000000 ) ) ;
#16748 = LINE ( 'NONE', #9665, #13023 ) ;
#16749 = AXIS2_PLACEMENT_3D ( 'NONE', #18587, #22595, #5874 ) ;
#16750 = DIRECTION ( 'NONE',  ( -0.000000000000000000, -0.000000000000000000, -1.000000000000000000 ) ) ;
#16751 = DIRECTION ( 'NONE',  ( 0.5579568342432839056, 0.8298699724180966797, 0.000000000000000000 ) ) ;
#16752 = CARTESIAN_POINT ( 'NONE',  ( 41.00000000000000000, 0.000000000000000000, 12.00000000000000000 ) ) ;
#16753 = ORIENTED_EDGE ( 'NONE', *, *, #2010, .T. ) ;
#16754 = CARTESIAN_POINT ( 'NONE',  ( 7.022953521754877748, 5.102474405760673903, 4.833165578109188232 ) ) ;
#16755 = EDGE_CURVE ( 'NONE', #17856, #13312, #20277, .T. ) ;
#16756 = VERTEX_POINT ( 'NONE', #12709 ) ;
#16757 = SHAPE_DEFINITION_REPRESENTATION ( #21913, #7043 ) ;
#16758 = ADVANCED_FACE ( 'NONE', ( #18577 ), #23944, .F. ) ;
#16759 = ORIENTED_EDGE ( 'NONE', *, *, #15224, .F. ) ;
#16760 = VERTEX_POINT ( 'NONE', #22233 ) ;
#16761 = ADVANCED_FACE ( 'NONE', ( #1853 ), #7092, .T. ) ;
#16762 = CYLINDRICAL_SURFACE ( 'NONE', #10319, 4.999999999999997335 ) ;
#16763 = CARTESIAN_POINT ( 'NONE',  ( -5.365059087798939252, -7.384370330707086261, -9.933165578109189653 ) ) ;
#16764 = ADVANCED_FACE ( 'NONE', ( #23712 ), #5398, .T. ) ;
#16765 = AXIS2_PLACEMENT_3D ( 'NONE', #19487, #8600, #21684 ) ;
#16766 = ORIENTED_EDGE ( 'NONE', *, *, #7085, .T. ) ;
#16767 = DIRECTION ( 'NONE',  ( 1.000000000000000000, 6.811450227741984732E-14, 0.000000000000000000 ) ) ;
#16768 = DIRECTION ( 'NONE',  ( 1.000000000000000000, 0.000000000000000000, -1.445602896647339163E-16 ) ) ;
#16769 = DIRECTION ( 'NONE',  ( 0.7089874389501501506, 0.7052211081716905916, 0.000000000000000000 ) ) ;
#16770 = PRODUCT_DEFINITION_SHAPE ( 'NONE', 'NONE',  #24112 ) ;
#16771 = FACE_OUTER_BOUND ( 'NONE', #10514, .T. ) ;
#16772 = DIRECTION ( 'NONE',  ( -1.000000000000000000, 0.000000000000000000, 0.000000000000000000 ) ) ;
#16773 = ORIENTED_EDGE ( 'NONE', *, *, #2974, .F. ) ;
#16774 = LINE ( 'NONE', #18270, #3617 ) ;
#16775 = EDGE_LOOP ( 'NONE', ( #9973, #8828, #7036, #9861, #17264, #7367 ) ) ;
#16776 = ORIENTED_EDGE ( 'NONE', *, *, #10812, .T. ) ;
#16777 = DIRECTION ( 'NONE',  ( 0.000000000000000000, -1.000000000000000000, 0.000000000000000000 ) ) ;
#16778 = CARTESIAN_POINT ( 'NONE',  ( -5.871322893124554021, 8.081182679343978492, -8.759589141758144848 ) ) ;
#16779 = CARTESIAN_POINT ( 'NONE',  ( -41.00000000000000000, 26.23076770084981391, 12.00000000000000000 ) ) ;
#16780 = CARTESIAN_POINT ( 'NONE',  ( 29.00000000000000000, -29.50000000000000355, 11.50000000000000000 ) ) ;
#16781 = CARTESIAN_POINT ( 'NONE',  ( 0.000000000000000000, 45.00000000000000000, -3.000000000000000000 ) ) ;
#16782 = CARTESIAN_POINT ( 'NONE',  ( 7.022953521755574080, -5.102474405759714671, -12.43316557810918788 ) ) ;
#16783 = CARTESIAN_POINT ( 'NONE',  ( 23.00000000000000000, -0.09016380984455869829, -11.68615217844040721 ) ) ;
#16784 = VERTEX_POINT ( 'NONE', #5503 ) ;
#16785 = EDGE_CURVE ( 'NONE', #18828, #3216, #6875, .T. ) ;
#16786 = ORIENTED_EDGE ( 'NONE', *, *, #13421, .F. ) ;
#16787=STYLED_ITEM('',(#24162),#18892);
#16788 = ORIENTED_EDGE ( 'NONE', *, *, #23896, .F. ) ;
#16789 = CIRCLE ( 'NONE', #6285, 2.000000000000000000 ) ;
#16790 = ORIENTED_EDGE ( 'NONE', *, *, #14745, .F. ) ;
#16791 = EDGE_CURVE ( 'NONE', #21962, #4241, #8728, .T. ) ;
#16792 = DIRECTION ( 'NONE',  ( 0.000000000000000000, -1.000000000000000000, 0.000000000000000000 ) ) ;
#16793 = DIRECTION ( 'NONE',  ( -0.5735764363510519326, 0.8191520442889876907, 1.003171929053519816E-16 ) ) ;
#16794 = EDGE_CURVE ( 'NONE', #19325, #20363, #5656, .T. ) ;
#16795 = DIRECTION ( 'NONE',  ( 0.000000000000000000, 0.000000000000000000, -1.000000000000000000 ) ) ;
#16796 = CARTESIAN_POINT ( 'NONE',  ( -42.00000000000000711, 26.82133436441678498, 11.00000000000000000 ) ) ;
#16797 = DIRECTION ( 'NONE',  ( 0.000000000000000000, 0.000000000000000000, 1.000000000000000000 ) ) ;
#16798 = LINE ( 'NONE', #5730, #1262 ) ;
#16799 = ORIENTED_EDGE ( 'NONE', *, *, #21323, .F. ) ;
#16800 = CIRCLE ( 'NONE', #12927, 1.500000000000000000 ) ;
#16801 = CARTESIAN_POINT ( 'NONE',  ( -23.84999999999999432, -15.03999999999999915, -25.00000000000000000 ) ) ;
#16802 = CARTESIAN_POINT ( 'NONE',  ( -29.00000000000000000, 29.49999999999999645, 11.50000000000000000 ) ) ;
#16803 = AXIS2_PLACEMENT_3D ( 'NONE', #21793, #6784, #3118 ) ;
#16804 = DIRECTION ( 'NONE',  ( -0.000000000000000000, -0.000000000000000000, -1.000000000000000000 ) ) ;
#16805 = CARTESIAN_POINT ( 'NONE',  ( 5.871322893124551356, -8.081182679343980269, 4.906742014460232504 ) ) ;
#16806 = ORIENTED_EDGE ( 'NONE', *, *, #2362, .F. ) ;
#16807 = ORIENTED_EDGE ( 'NONE', *, *, #6203, .F. ) ;
#16808 = CARTESIAN_POINT ( 'NONE',  ( -9.500000000000000000, 0.000000000000000000, 12.50000000000000000 ) ) ;
#16809 = ORIENTED_EDGE ( 'NONE', *, *, #6233, .T. ) ;
#16810 = EDGE_CURVE ( 'NONE', #13616, #47, #3552, .T. ) ;
#16811 = EDGE_LOOP ( 'NONE', ( #23893, #19816 ) ) ;
#16812 = CARTESIAN_POINT ( 'NONE',  ( 5.378177448618336243, 0.000000000000000000, 0.000000000000000000 ) ) ;
#16813 = CARTESIAN_POINT ( 'NONE',  ( 39.00000000000000000, 28.80990663662251805, 11.00000000000000000 ) ) ;
#16814 = CIRCLE ( 'NONE', #4375, 5.000000000000007994 ) ;
#16815 = CARTESIAN_POINT ( 'NONE',  ( -31.74999999999995737, 0.000000000000000000, 0.000000000000000000 ) ) ;
#16816 = AXIS2_PLACEMENT_3D ( 'NONE', #9716, #13763, #13396 ) ;
#16817 = EDGE_CURVE ( 'NONE', #23927, #20733, #7198, .T. ) ;
#16818 = VECTOR ( 'NONE', #5138, 1000.000000000000000 ) ;
#16819 = VECTOR ( 'NONE', #22210, 1000.000000000000000 ) ;
#16820 = DIRECTION ( 'NONE',  ( 0.000000000000000000, -1.000000000000000000, 0.000000000000000000 ) ) ;
#16821 = EDGE_CURVE ( 'NONE', #2607, #14074, #16255, .T. ) ;
#16822 = VECTOR ( 'NONE', #11577, 1000.000000000000000 ) ;
#16823 = CIRCLE ( 'NONE', #23087, 4.172000000000008590 ) ;
#16824 = CIRCLE ( 'NONE', #7866, 1.499999999999994449 ) ;
#16825 = CARTESIAN_POINT ( 'NONE',  ( -9.499999999999790390, -3.086737114213257804, -5.159589141758141650 ) ) ;
#16826 = EDGE_LOOP ( 'NONE', ( #792, #19587, #5744, #13041 ) ) ;
#16827 = CARTESIAN_POINT ( 'NONE',  ( 33.99999999999998579, -5.000000000000013323, 10.49999999999999822 ) ) ;
#16828 = DIRECTION ( 'NONE',  ( 0.000000000000000000, -0.000000000000000000, -1.000000000000000000 ) ) ;
#16829 = VERTEX_POINT ( 'NONE', #16827 ) ;
#16830 = DIRECTION ( 'NONE',  ( -1.000000000000000000, -1.224606353822377258E-16, -0.000000000000000000 ) ) ;
#16831 = DIRECTION ( 'NONE',  ( 0.000000000000000000, 0.000000000000000000, -1.000000000000000000 ) ) ;
#16832 = AXIS2_PLACEMENT_3D ( 'NONE', #17661, #10564, #8390 ) ;
#16833 = AXIS2_PLACEMENT_3D ( 'NONE', #19314, #12924, #24049 ) ;
#16834 = CARTESIAN_POINT ( 'NONE',  ( -2.259833726595073422, 8.712823366420707316, 79.01727130922115805 ) ) ;
#16835 = VECTOR ( 'NONE', #12545, 1000.000000000000000 ) ;
#16836 = EDGE_CURVE ( 'NONE', #23135, #3028, #599, .T. ) ;
#16837 = PLANE ( 'NONE',  #10994 ) ;
#16838 = AXIS2_PLACEMENT_3D ( 'NONE', #1931, #11062, #14490 ) ;
#16839 = DIRECTION ( 'NONE',  ( 1.000000000000000000, 0.000000000000000000, 0.000000000000000000 ) ) ;
#16840 = AXIS2_PLACEMENT_3D ( 'NONE', #11589, #17086, #2452 ) ;
#16841 = DIRECTION ( 'NONE',  ( -1.000000000000000000, -0.000000000000000000, -0.000000000000000000 ) ) ;
#16842 = ORIENTED_EDGE ( 'NONE', *, *, #22417, .T. ) ;
#16843 = CIRCLE ( 'NONE', #6343, 5.000000000000007994 ) ;
#16844 = CARTESIAN_POINT ( 'NONE',  ( -3.008080266967722682, 45.00000000000000000, 0.000000000000000000 ) ) ;
#16845 = EDGE_CURVE ( 'NONE', #10814, #14, #10687, .T. ) ;
#16846 = CARTESIAN_POINT ( 'NONE',  ( -28.99999999999999645, 29.50000000000000000, 27.00000000000000000 ) ) ;
#16847 = CIRCLE ( 'NONE', #518, 0.2999999999999999334 ) ;
#16848 = CARTESIAN_POINT ( 'NONE',  ( 70.51113724927145654, 7.420530141404717394E-15, 0.000000000000000000 ) ) ;
#16849 = ADVANCED_FACE ( 'NONE', ( #22354 ), #832, .T. ) ;
#16850 = CARTESIAN_POINT ( 'NONE',  ( 4.489900896931573904, 0.000000000000000000, 0.000000000000000000 ) ) ;
#16851 = EDGE_LOOP ( 'NONE', ( #14131, #15655 ) ) ;
#16852 = VERTEX_POINT ( 'NONE', #15464 ) ;
#16853 = EDGE_LOOP ( 'NONE', ( #17641, #529, #13760, #16154 ) ) ;
#16854 = VECTOR ( 'NONE', #15006, 1000.000000000000000 ) ;
#16855 = ORIENTED_EDGE ( 'NONE', *, *, #16439, .F. ) ;
#16857 = VECTOR ( 'NONE', #4267, 1000.000000000000000 ) ;
#16856 = DIRECTION ( 'NONE',  ( 0.000000000000000000, 0.000000000000000000, -1.000000000000000000 ) ) ;
#16858 = DIRECTION ( 'NONE',  ( 1.000000000000000000, 0.000000000000000000, 0.000000000000000000 ) ) ;
#16859 = CONICAL_SURFACE ( 'NONE', #20009, 2.024999999999999911, 0.7853981633974743692 ) ;
#16860 = CIRCLE ( 'NONE', #9450, 2.000000000000000000 ) ;
#16861 = DIRECTION ( 'NONE',  ( -1.000000000000000000, -0.000000000000000000, -0.000000000000000000 ) ) ;
#16862 = ORIENTED_EDGE ( 'NONE', *, *, #5135, .F. ) ;
#16863 = AXIS2_PLACEMENT_3D ( 'NONE', #22367, #16841, #20763 ) ;
#16864 = DIRECTION ( 'NONE',  ( -1.000000000000000000, 0.000000000000000000, 0.000000000000000000 ) ) ;
#16865 = CIRCLE ( 'NONE', #21171, 8.000000000000000000 ) ;
#16866 = ORIENTED_EDGE ( 'NONE', *, *, #18346, .T. ) ;
#16867 = PRODUCT_RELATED_PRODUCT_CATEGORY ( 'part', '', ( #18223 ) ) ;
#16868 = LINE ( 'NONE', #9549, #17598 ) ;
#16869 = LINE ( 'NONE', #188, #12162 ) ;
#16870 = CARTESIAN_POINT ( 'NONE',  ( -33.24999999999999289, 29.50000000000000000, -3.000000000000000000 ) ) ;
#16871 = CARTESIAN_POINT ( 'NONE',  ( 9.500000000000000000, 1.163414459189985485E-15, 12.50000000000000000 ) ) ;
#16872 = ORIENTED_EDGE ( 'NONE', *, *, #19540, .T. ) ;
#16873 = AXIS2_PLACEMENT_3D ( 'NONE', #3653, #22327, #23915 ) ;
#16874 = CARTESIAN_POINT ( 'NONE',  ( -23.85000000000000497, 15.03999999999999915, -25.00000000000000000 ) ) ;
#16875 = EDGE_CURVE ( 'NONE', #13484, #13330, #20852, .T. ) ;
#16876 = DIRECTION ( 'NONE',  ( -1.000000000000000000, -1.224606353822377258E-16, -0.000000000000000000 ) ) ;
#16877 = EDGE_CURVE ( 'NONE', #11051, #2739, #2411, .T. ) ;
#16878 = VERTEX_POINT ( 'NONE', #12031 ) ;
#16879 = VECTOR ( 'NONE', #21648, 1000.000000000000000 ) ;
#16880 = AXIS2_PLACEMENT_3D ( 'NONE', #11984, #544, #19207 ) ;
#16881 = VERTEX_POINT ( 'NONE', #15574 ) ;
#16882 = CARTESIAN_POINT ( 'NONE',  ( 9.500000000000000000, 6.470877716354879437E-13, 12.05958914175814378 ) ) ;
#16883 = ORIENTED_EDGE ( 'NONE', *, *, #19440, .F. ) ;
#16884 = AXIS2_PLACEMENT_3D ( 'NONE', #22766, #15165, #9320 ) ;
#16885 = AXIS2_PLACEMENT_3D ( 'NONE', #12465, #6754, #23474 ) ;
#16886 = AXIS2_PLACEMENT_3D ( 'NONE', #9915, #2731, #786 ) ;
#16887 = CIRCLE ( 'NONE', #6390, 5.000000000000007994 ) ;
#16888 = EDGE_LOOP ( 'NONE', ( #5445, #15717, #18105, #23943 ) ) ;
#16889 = VERTEX_POINT ( 'NONE', #22927 ) ;
#16890 = CARTESIAN_POINT ( 'NONE',  ( -28.99999999999999645, 29.50000000000000000, -3.000000000000000000 ) ) ;
#16891 = CARTESIAN_POINT ( 'NONE',  ( -5.365059087799947335, 7.384370330706355290, -11.33316557810918468 ) ) ;
#16892 = DIRECTION ( 'NONE',  ( -1.000000000000000000, -1.224606353822377258E-16, -0.000000000000000000 ) ) ;
#16893 = ORIENTED_EDGE ( 'NONE', *, *, #18496, .F. ) ;
#16894 = LINE ( 'NONE', #209, #5244 ) ;
#16895 = CARTESIAN_POINT ( 'NONE',  ( 23.00000000000000000, -13.66196005206961850, 2.131329562388824428 ) ) ;
#16896 = CARTESIAN_POINT ( 'NONE',  ( 0.000000000000000000, 0.000000000000000000, 3.699999999999998845 ) ) ;
#16897 = LINE ( 'NONE', #20330, #7184 ) ;
#16898 = PRODUCT_DEFINITION ( 'UNKNOWN', '', #9195, #6027 ) ;
#16899 = DIRECTION ( 'NONE',  ( 0.5735764363510427177, -0.8191520442889941300, 1.003171929053527705E-16 ) ) ;
#16900 = VERTEX_POINT ( 'NONE', #4373 ) ;
#16901 = CARTESIAN_POINT ( 'NONE',  ( 0.000000000000000000, 0.000000000000000000, 12.50000000000000000 ) ) ;
#16902 = EDGE_CURVE ( 'NONE', #8545, #23927, #592, .T. ) ;
#16903 = AXIS2_PLACEMENT_3D ( 'NONE', #11572, #13656, #8408 ) ;
#16904 = AXIS2_PLACEMENT_3D ( 'NONE', #22136, #19825, #12591 ) ;
#16905 = ORIENTED_EDGE ( 'NONE', *, *, #12668, .T. ) ;
#16906 = CIRCLE ( 'NONE', #11440, 5.000000000000007994 ) ;
#16907 = CARTESIAN_POINT ( 'NONE',  ( 30.44534269664590553, 40.40463133211080304, 0.000000000000000000 ) ) ;
#16908 = CARTESIAN_POINT ( 'NONE',  ( 0.000000000000000000, -13.61176534793443338, -4.089617900950226925 ) ) ;
#16909 = CONICAL_SURFACE ( 'NONE', #12244, 7.999999999999992895, 0.7853981633974439491 ) ;
#16910 = DIRECTION ( 'NONE',  ( -1.000000000000000000, -1.224606353822377258E-16, -0.000000000000000000 ) ) ;
#16911 = CARTESIAN_POINT ( 'NONE',  ( 17.06033556854819011, 8.068938288216807919, -5.036196554528634017 ) ) ;
#16912 = VECTOR ( 'NONE', #19645, 1000.000000000000000 ) ;
#16913 = DIRECTION ( 'NONE',  ( 0.000000000000000000, 0.000000000000000000, -1.000000000000000000 ) ) ;
#16914 = ADVANCED_FACE ( 'NONE', ( #2664 ), #6034, .T. ) ;
#16915 = FACE_OUTER_BOUND ( 'NONE', #21292, .T. ) ;
#16916 = EDGE_CURVE ( 'NONE', #747, #19039, #16373, .T. ) ;
#16917 = CARTESIAN_POINT ( 'NONE',  ( -9.500000000000000000, -6.482511860946779655E-13, 8.206742014460234103 ) ) ;
#16918 = ORIENTED_EDGE ( 'NONE', *, *, #19336, .F. ) ;
#16919 = ORIENTED_EDGE ( 'NONE', *, *, #20282, .T. ) ;
#16920 = EDGE_LOOP ( 'NONE', ( #6013, #19124, #6412, #17546 ) ) ;
#16921 = ORIENTED_EDGE ( 'NONE', *, *, #8221, .T. ) ;
#16922 = CIRCLE ( 'NONE', #20827, 5.000000000000007994 ) ;
#16923 = AXIS2_PLACEMENT_3D ( 'NONE', #20794, #9306, #16651 ) ;
#16924 = ORIENTED_EDGE ( 'NONE', *, *, #16152, .F. ) ;
#16925 = CARTESIAN_POINT ( 'NONE',  ( -7.685661446561619314, -5.583959896779019161, 9.259589141758143072 ) ) ;
#16926 = AXIS2_PLACEMENT_3D ( 'NONE', #20699, #7857, #15181 ) ;
#16927 = CIRCLE ( 'NONE', #3686, 1.000000000000000888 ) ;
#16928 = CARTESIAN_POINT ( 'NONE',  ( -28.99999999999998579, -29.50000000000000711, 0.000000000000000000 ) ) ;
#16929 = LINE ( 'NONE', #13524, #22835 ) ;
#16930 = DIRECTION ( 'NONE',  ( 0.000000000000000000, 0.000000000000000000, 1.000000000000000000 ) ) ;
#16931 = AXIS2_PLACEMENT_3D ( 'NONE', #13520, #4248, #21070 ) ;
#16932 = CARTESIAN_POINT ( 'NONE',  ( 9.500000000000000000, 6.470877716354879437E-13, -10.05958914175814378 ) ) ;
#16933 = EDGE_CURVE ( 'NONE', #6874, #7931, #13062, .T. ) ;
#16934 = ORIENTED_EDGE ( 'NONE', *, *, #1253, .T. ) ;
#16935 = CARTESIAN_POINT ( 'NONE',  ( 0.000000000000000000, 0.000000000000000000, 12.50000000000000000 ) ) ;
#16936 = SURFACE_SIDE_STYLE ('',( #9478 ) ) ;
#16937 = CYLINDRICAL_SURFACE ( 'NONE', #17615, 17.87500000001787726 ) ;
#16938 = CARTESIAN_POINT ( 'NONE',  ( -17.38971744193260349, 8.915620082851750894, 3.315798060087249421 ) ) ;
#16939 = APPLICATION_CONTEXT ( 'automotive_design' ) ;
#16940 = LINE ( 'NONE', #254, #19266 ) ;
#16941 = ADVANCED_FACE ( 'NONE', ( #21211 ), #21340, .T. ) ;
#16942 = VERTEX_POINT ( 'NONE', #8246 ) ;
#16943 = ADVANCED_FACE ( 'NONE', ( #19390 ), #3307, .T. ) ;
#16944 = CARTESIAN_POINT ( 'NONE',  ( 6.699999999999999289, 0.000000000000000000, 0.000000000000000000 ) ) ;
#16945 = VERTEX_POINT ( 'NONE', #15706 ) ;
#16946 = CARTESIAN_POINT ( 'NONE',  ( -2.999999999999996447, 111.0000000000000000, 98.99999999999998579 ) ) ;
#16947 = CONICAL_SURFACE ( 'NONE', #22799, 39.49999999999999289, 0.7853981633974621568 ) ;
#16948 = VERTEX_POINT ( 'NONE', #7555 ) ;
#16949 = CARTESIAN_POINT ( 'NONE',  ( -7.685661446561619314, -5.583959896779019161, -9.259589141758143072 ) ) ;
#16950 = ORIENTED_EDGE ( 'NONE', *, *, #18579, .T. ) ;
#16951 = CONICAL_SURFACE ( 'NONE', #617, 10.50249999999999950, 0.7853981633974447263 ) ;
#16952 = VECTOR ( 'NONE', #8748, 1000.000000000000000 ) ;
#16953 = CARTESIAN_POINT ( 'NONE',  ( 5.000000000000000000, 4.685197434473818312, -1.301042606982605321E-15 ) ) ;
#16954 = DIRECTION ( 'NONE',  ( 0.000000000000000000, 0.000000000000000000, -1.000000000000000000 ) ) ;
#16955 = CARTESIAN_POINT ( 'NONE',  ( 87.67068093254673045, 7.562528597612068045E-15, 0.000000000000000000 ) ) ;
#16956 = DIRECTION ( 'NONE',  ( -1.000000000000000000, -0.000000000000000000, -0.000000000000000000 ) ) ;
#16957 = CARTESIAN_POINT ( 'NONE',  ( -6.822232771736903637E-13, 9.988891130263535700, -10.55958914175814378 ) ) ;
#16958 = VERTEX_POINT ( 'NONE', #23171 ) ;
#16959 = AXIS2_PLACEMENT_3D ( 'NONE', #12928, #16599, #12696 ) ;
#16960 = CARTESIAN_POINT ( 'NONE',  ( 76.90909090909090651, -4.172000000000000597, 5.616230220889771312E-16 ) ) ;
#16961 = AXIS2_PLACEMENT_3D ( 'NONE', #1540, #18607, #2148 ) ;
#16962 = ORIENTED_EDGE ( 'NONE', *, *, #20182, .T. ) ;
#16963 = CARTESIAN_POINT ( 'NONE',  ( 78.36363636363637397, -4.172000000000000597, 0.000000000000000000 ) ) ;
#16964 = CARTESIAN_POINT ( 'NONE',  ( 1.845666383292525525, 8.813255204463377623, 78.60324786774314987 ) ) ;
#16965 = FACE_BOUND ( 'NONE', #23330, .T. ) ;
#16966 = AXIS2_PLACEMENT_3D ( 'NONE', #422, #7720, #15154 ) ;
#16967 = CARTESIAN_POINT ( 'NONE',  ( 42.00000000000000000, 25.22443390181681622, -1.500000000000000000 ) ) ;
#16968 = CARTESIAN_POINT ( 'NONE',  ( 44.99999999999998579, 50.99999999999992184, 0.000000000000000000 ) ) ;
#16969 = ADVANCED_FACE ( 'NONE', ( #6453 ), #23963, .F. ) ;
#16970 = CARTESIAN_POINT ( 'NONE',  ( -21.84999999999999787, 0.000000000000000000, 12.00000000000000000 ) ) ;
#16971 = CARTESIAN_POINT ( 'NONE',  ( 10.00000000000000178, 0.000000000000000000, 0.000000000000000000 ) ) ;
#16972 = CARTESIAN_POINT ( 'NONE',  ( -2.983080266967717442, 45.00000000000000000, 0.02500000000000418554 ) ) ;
#16973 = ORIENTED_EDGE ( 'NONE', *, *, #3345, .T. ) ;
#16974 = CARTESIAN_POINT ( 'NONE',  ( 34.02499999999999858, 29.50000000000000000, -3.000000000000000000 ) ) ;
#16975 = DIRECTION ( 'NONE',  ( -1.000000000000000000, -1.387778780781445478E-15, 0.000000000000000000 ) ) ;
#16976 = CYLINDRICAL_SURFACE ( 'NONE', #18573, 8.000000000000000000 ) ;
#16977 = VECTOR ( 'NONE', #22415, 1000.000000000000000 ) ;
#16978 = DIRECTION ( 'NONE',  ( -1.000000000000000000, -1.224606353822377258E-16, -0.000000000000000000 ) ) ;
#16979 = AXIS2_PLACEMENT_3D ( 'NONE', #10585, #7299, #1353 ) ;
#16980 = FACE_OUTER_BOUND ( 'NONE', #15517, .T. ) ;
#16981 = ORIENTED_EDGE ( 'NONE', *, *, #3093, .T. ) ;
#16982 = PRODUCT_DEFINITION_SHAPE ( 'NONE', 'NONE',  #5009 ) ;
#16983 = EDGE_LOOP ( 'NONE', ( #1758, #4978, #7173, #1360, #4300 ) ) ;
#16984 = ORIENTED_EDGE ( 'NONE', *, *, #19182, .F. ) ;
#16985 = CARTESIAN_POINT ( 'NONE',  ( 10.40000000000000036, 0.000000000000000000, -5.400000000000001243 ) ) ;
#16986 = ADVANCED_FACE ( 'NONE', ( #20527 ), #3800, .F. ) ;
#16987 = CARTESIAN_POINT ( 'NONE',  ( 5.871322893123448239, 8.081182679344781405, 9.506742014460231260 ) ) ;
#16988 = ORIENTED_EDGE ( 'NONE', *, *, #10211, .T. ) ;
#16989 = ORIENTED_EDGE ( 'NONE', *, *, #10657, .F. ) ;
#16990 = CARTESIAN_POINT ( 'NONE',  ( -9.378401895172221003, -4.713374146359802882E-16, -12.12159810482778788 ) ) ;
#16991 = EDGE_CURVE ( 'NONE', #23864, #1818, #19280, .T. ) ;
#16992 = CONICAL_SURFACE ( 'NONE', #13508, 4.172000000000008590, 0.9599310885968742602 ) ;
#16993 = DIRECTION ( 'NONE',  ( 0.8298699724180977899, 0.5579568342432823513, -0.000000000000000000 ) ) ;
#16994 = ORIENTED_EDGE ( 'NONE', *, *, #15623, .F. ) ;
#16995 = CARTESIAN_POINT ( 'NONE',  ( -7.957653757147100215, -5.196064979199609191, -3.501362371312797706 ) ) ;
#16996 = EDGE_CURVE ( 'NONE', #3894, #5827, #4121, .T. ) ;
#16997 = AXIS2_PLACEMENT_3D ( 'NONE', #17257, #9682, #7843 ) ;
#16998 = EDGE_CURVE ( 'NONE', #16379, #21962, #20469, .T. ) ;
#16999 = ORIENTED_EDGE ( 'NONE', *, *, #787, .F. ) ;
#17000 = CARTESIAN_POINT ( 'NONE',  ( -29.00000000000000000, -3.851859888774471706E-31, 10.49999999999999822 ) ) ;
#17001 = LINE ( 'NONE', #7593, #15726 ) ;
#17002 = CIRCLE ( 'NONE', #13517, 11.68650000001168721 ) ;
#17003 = CARTESIAN_POINT ( 'NONE',  ( -31.10231664966676846, 45.36128193761570770, 11.00000000000000000 ) ) ;
#17004 = LINE ( 'NONE', #13335, #1750 ) ;
#17005 = ORIENTED_EDGE ( 'NONE', *, *, #320, .T. ) ;
#17006 = FACE_BOUND ( 'NONE', #83, .T. ) ;
#17007 = CARTESIAN_POINT ( 'NONE',  ( 28.73477696352899713, 42.73830357953205095, -1.500000000000000000 ) ) ;
#17008 = EDGE_LOOP ( 'NONE', ( #17920, #13890, #6880, #18445 ) ) ;
#17009 = CARTESIAN_POINT ( 'NONE',  ( -5.365059087799947335, 7.384370330706355290, 5.333165578109189120 ) ) ;
#17010 = ORIENTED_EDGE ( 'NONE', *, *, #22569, .T. ) ;
#17011 = CIRCLE ( 'NONE', #8452, 4.249999999999996447 ) ;
#17012 = APPLICATION_PROTOCOL_DEFINITION ( 'draft international standard', 'automotive_design', 1998, #6527 ) ;
#17013 = CYLINDRICAL_SURFACE ( 'NONE', #3758, 18.50000000000000000 ) ;
#17014 = ORIENTED_EDGE ( 'NONE', *, *, #186, .F. ) ;
#17015 = ORIENTED_EDGE ( 'NONE', *, *, #17396, .F. ) ;
#17016 = DIRECTION ( 'NONE',  ( 1.000000000000000000, 0.000000000000000000, 0.000000000000000000 ) ) ;
#17017 = CARTESIAN_POINT ( 'NONE',  ( 5.365059087798938364, 7.384370330707087149, -10.93316557810918788 ) ) ;
#17018 = SHAPE_REPRESENTATION ( 'Part10^Assembly Drive shaft gear', ( #8005 ), #7613 ) ;
#17019 = CARTESIAN_POINT ( 'NONE',  ( 4.489900896931573904, 1.040949779275250140E-15, 8.500000000000000000 ) ) ;
#17020 = ORIENTED_EDGE ( 'NONE', *, *, #15576, .F. ) ;
#17021 = CARTESIAN_POINT ( 'NONE',  ( -36.00000000000000711, -51.00000000000000711, 0.000000000000000000 ) ) ;
#17022 = FACE_OUTER_BOUND ( 'NONE', #18067, .T. ) ;
#17023 = FACE_OUTER_BOUND ( 'NONE', #7025, .T. ) ;
#17024 = EDGE_CURVE ( 'NONE', #5490, #16784, #1918, .T. ) ;
#17025 = ADVANCED_FACE ( 'NONE', ( #17148 ), #13377, .F. ) ;
#17026 = CARTESIAN_POINT ( 'NONE',  ( 23.00000000000000000, 12.00453763395396756, -7.608955687739546114 ) ) ;
#17027 = ORIENTED_EDGE ( 'NONE', *, *, #3412, .T. ) ;
#17028 = FACE_OUTER_BOUND ( 'NONE', #11514, .T. ) ;
#17029 = ORIENTED_EDGE ( 'NONE', *, *, #14382, .T. ) ;
#17030 = DIRECTION ( 'NONE',  ( -0.000000000000000000, -0.000000000000000000, -1.000000000000000000 ) ) ;
#17031 = CARTESIAN_POINT ( 'NONE',  ( 2.935661446561383503, 9.035036904804158553, -8.459589141758144137 ) ) ;
#17032 = CARTESIAN_POINT ( 'NONE',  ( -40.66734255040736201, -26.56420859267092283, -3.000000000000000000 ) ) ;
#17033 = LINE ( 'NONE', #18747, #3677 ) ;
#17034 = DIRECTION ( 'NONE',  ( 0.000000000000000000, 0.000000000000000000, 1.000000000000000000 ) ) ;
#17035 = CARTESIAN_POINT ( 'NONE',  ( -2.682529543900285862, 8.255977015246234174, -11.23316557810918859 ) ) ;
#17036 = PRESENTATION_STYLE_ASSIGNMENT (( #6188 ) ) ;
#17037 = ORIENTED_EDGE ( 'NONE', *, *, #4799, .F. ) ;
#17038 = ORIENTED_EDGE ( 'NONE', *, *, #11805, .T. ) ;
#17039 = VECTOR ( 'NONE', #13952, 1000.000000000000000 ) ;
#17040 = EDGE_LOOP ( 'NONE', ( #4757, #2017, #19911, #13709 ) ) ;
#17041 = LINE ( 'NONE', #15082, #19072 ) ;
#17042 = ORIENTED_EDGE ( 'NONE', *, *, #20070, .T. ) ;
#17043 = DIRECTION ( 'NONE',  ( 1.000000000000000000, 0.000000000000000000, 0.000000000000000000 ) ) ;
#17044 = CARTESIAN_POINT ( 'NONE',  ( -9.500000000000000000, 0.000000000000000000, 12.50000000000000000 ) ) ;
#17045 = CIRCLE ( 'NONE', #23317, 10.00000000000000533 ) ;
#17046 = ADVANCED_FACE ( 'NONE', ( #18638 ), #13824, .T. ) ;
#17047 = VECTOR ( 'NONE', #20196, 1000.000000000000000 ) ;
#17048 = CARTESIAN_POINT ( 'NONE',  ( 0.000000000000000000, -45.00000000000000000, 27.00000000000000000 ) ) ;
#17049 = DIRECTION ( 'NONE',  ( -1.000000000000000000, -0.000000000000000000, -0.000000000000000000 ) ) ;
#17050 = SURFACE_STYLE_FILL_AREA ( #239 ) ;
#17051 = LINE ( 'NONE', #6542, #11768 ) ;
#17052 = EDGE_CURVE ( 'NONE', #18218, #19938, #18886, .T. ) ;
#17053 = EDGE_CURVE ( 'NONE', #16134, #15497, #22432, .T. ) ;
#17054 = LINE ( 'NONE', #7765, #5935 ) ;
#17055 = CARTESIAN_POINT ( 'NONE',  ( 0.000000000000000000, 0.000000000000000000, -27.00000000000000000 ) ) ;
#17056 = CARTESIAN_POINT ( 'NONE',  ( 71.09090909090909349, -4.172000000000000597, 0.000000000000000000 ) ) ;
#17057 = CARTESIAN_POINT ( 'NONE',  ( -15.57833309066360705, 5.219313726039665369, -7.987432870209370428 ) ) ;
#17058 = FACE_OUTER_BOUND ( 'NONE', #20067, .T. ) ;
#17059 = EDGE_LOOP ( 'NONE', ( #19226, #17809, #10418, #22917 ) ) ;
#17060 = AXIS2_PLACEMENT_3D ( 'NONE', #11639, #1908, #9797 ) ;
#17061 = DIRECTION ( 'NONE',  ( -0.7071067811865292541, 0.000000000000000000, -0.7071067811865658914 ) ) ;
#17062 = CIRCLE ( 'NONE', #17077, 6.050000000006050982 ) ;
#17063 = ORIENTED_EDGE ( 'NONE', *, *, #5132, .T. ) ;
#17064 = LINE ( 'NONE', #4018, #4084 ) ;
#17065 = EDGE_LOOP ( 'NONE', ( #46, #24095, #14423, #10597 ) ) ;
#17066 = PLANE ( 'NONE',  #14145 ) ;
#17067 = ORIENTED_EDGE ( 'NONE', *, *, #19184, .T. ) ;
#17068 = ADVANCED_FACE ( 'NONE', ( #11402 ), #22652, .F. ) ;
#17069 = LINE ( 'NONE', #7546, #15679 ) ;
#17070 = CARTESIAN_POINT ( 'NONE',  ( 20.85000000000000497, 16.67999999999999972, 13.00000000000000178 ) ) ;
#17071 = CARTESIAN_POINT ( 'NONE',  ( 0.000000000000000000, 0.000000000000000000, 12.50000000000000000 ) ) ;
#17072 = AXIS2_PLACEMENT_3D ( 'NONE', #14581, #16295, #23755 ) ;
#17073 = CARTESIAN_POINT ( 'NONE',  ( 4.379988124296556151, -7.836644668421599569, -12.50000000000000355 ) ) ;
#17074 = CYLINDRICAL_SURFACE ( 'NONE', #14493, 9.000000000000000000 ) ;
#17075 = ADVANCED_FACE ( 'NONE', ( #99 ), #11852, .T. ) ;
#17076 = EDGE_CURVE ( 'NONE', #21352, #3705, #981, .T. ) ;
#17077 = AXIS2_PLACEMENT_3D ( 'NONE', #4044, #13294, #2214 ) ;
#17078 = FACE_OUTER_BOUND ( 'NONE', #14703, .T. ) ;
#17079 = ORIENTED_EDGE ( 'NONE', *, *, #14215, .F. ) ;
#17080 = ORIENTED_EDGE ( 'NONE', *, *, #2903, .T. ) ;
#17081 = DIRECTION ( 'NONE',  ( 0.000000000000000000, -1.000000000000000000, 9.256405414277000802E-16 ) ) ;
#17082 = DIRECTION ( 'NONE',  ( 0.000000000000000000, -1.000000000000000000, 0.000000000000000000 ) ) ;
#17083 = CYLINDRICAL_SURFACE ( 'NONE', #18264, 1.000000000000000888 ) ;
#17084 = FACE_OUTER_BOUND ( 'NONE', #7902, .T. ) ;
#17085 = CARTESIAN_POINT ( 'NONE',  ( -2.844348310502767152, 8.539081767371294873, 80.02643058434389900 ) ) ;
#17086 = DIRECTION ( 'NONE',  ( 0.000000000000000000, -0.000000000000000000, -1.000000000000000000 ) ) ;
#17087 = CARTESIAN_POINT ( 'NONE',  ( -29.00000000000000000, -29.49999999999999645, 11.50000000000000000 ) ) ;
#17088 = CARTESIAN_POINT ( 'NONE',  ( 40.23082370883258818, -29.49999999999999645, -3.000000000000000000 ) ) ;
#17089 = ORIENTED_EDGE ( 'NONE', *, *, #9581, .F. ) ;
#17090 = FACE_BOUND ( 'NONE', #7977, .T. ) ;
#17091 = CARTESIAN_POINT ( 'NONE',  ( 7.022953521754877748, 5.102474405760673903, 10.83316557810919001 ) ) ;
#17092 = CARTESIAN_POINT ( 'NONE',  ( -23.85000000000000497, 15.03999999999999915, -25.00000000000000000 ) ) ;
#17093 = CARTESIAN_POINT ( 'NONE',  ( 20.85000000000000497, 15.03999999999999737, 0.000000000000000000 ) ) ;
#17094 = PRESENTATION_LAYER_ASSIGNMENT (  '', '', ( #21406 ) ) ;
#17095 = ADVANCED_FACE ( 'NONE', ( #20837 ), #576, .T. ) ;
#17096 = CARTESIAN_POINT ( 'NONE',  ( 23.90000000000000568, 29.50000000000000355, 11.50000000000000000 ) ) ;
#17097 = EDGE_LOOP ( 'NONE', ( #4141, #21241, #19078, #583 ) ) ;
#17098 = ORIENTED_EDGE ( 'NONE', *, *, #8255, .T. ) ;
#17099 = ITEM_DEFINED_TRANSFORMATION ( 'NONE', 'NONE', #13489,  #5695 ) ;
#17100 = ORIENTED_EDGE ( 'NONE', *, *, #18665, .T. ) ;
#17101 = FACE_OUTER_BOUND ( 'NONE', #12097, .T. ) ;
#17102 = ADVANCED_FACE ( 'NONE', ( #3868 ), #11274, .F. ) ;
#17103 = EDGE_CURVE ( 'NONE', #14826, #15497, #4090, .T. ) ;
#17104 = CARTESIAN_POINT ( 'NONE',  ( -7.685661446562381371, 5.583959896777970222, -8.006742014460233037 ) ) ;
#17105 = ORIENTED_EDGE ( 'NONE', *, *, #5367, .F. ) ;
#17106 = DIRECTION ( 'NONE',  ( 1.000000000000000000, 0.000000000000000000, 0.000000000000000000 ) ) ;
#17107 = ORIENTED_EDGE ( 'NONE', *, *, #23440, .T. ) ;
#17108 = CARTESIAN_POINT ( 'NONE',  ( -5.733664283190738509, -7.594766265237401726, -3.500616659224041527 ) ) ;
#17109 =( REPRESENTATION_RELATIONSHIP ('NONE','NONE', #21748, #23456 ) REPRESENTATION_RELATIONSHIP_WITH_TRANSFORMATION ( #8178 )SHAPE_REPRESENTATION_RELATIONSHIP( ) );
#17110 = EDGE_LOOP ( 'NONE', ( #6813, #2228, #19398, #11733 ) ) ;
#17111 = CYLINDRICAL_SURFACE ( 'NONE', #7086, 9.499999999999994671 ) ;
#17112 = LINE ( 'NONE', #6024, #7101 ) ;
#17113 = CYLINDRICAL_SURFACE ( 'NONE', #19238, 17.87500000001787726 ) ;
#17114 = DIRECTION ( 'NONE',  ( 0.5801326495544486539, 0.000000000000000000, -0.8145220125453549453 ) ) ;
#17115 = ORIENTED_EDGE ( 'NONE', *, *, #18777, .T. ) ;
#17116 = DIRECTION ( 'NONE',  ( 4.613626265895764052E-16, -1.000000000000000000, 0.000000000000000000 ) ) ;
#17117 = DIRECTION ( 'NONE',  ( 0.000000000000000000, -0.000000000000000000, -1.000000000000000000 ) ) ;
#17118 = EDGE_CURVE ( 'NONE', #8089, #3765, #14965, .T. ) ;
#17119 = ORIENTED_EDGE ( 'NONE', *, *, #3081, .T. ) ;
#17120 = AXIS2_PLACEMENT_3D ( 'NONE', #21445, #4365, #11778 ) ;
#17121 = ORIENTED_EDGE ( 'NONE', *, *, #22386, .T. ) ;
#17122 = CARTESIAN_POINT ( 'NONE',  ( -5.365059087799947335, 7.384370330706355290, 3.333165578109187344 ) ) ;
#17123 = VERTEX_POINT ( 'NONE', #2523 ) ;
#17124 = AXIS2_PLACEMENT_3D ( 'NONE', #23017, #23278, #6551 ) ;
#17125 = EDGE_CURVE ( 'NONE', #14863, #23135, #23019, .T. ) ;
#17126 = ORIENTED_EDGE ( 'NONE', *, *, #17824, .T. ) ;
#17127 = LINE ( 'NONE', #1138, #9145 ) ;
#17128 = ORIENTED_EDGE ( 'NONE', *, *, #6127, .T. ) ;
#17129 = ORIENTED_EDGE ( 'NONE', *, *, #22418, .F. ) ;
#17130 = EDGE_CURVE ( 'NONE', #21134, #2764, #18510, .T. ) ;
#17131 = LINE ( 'NONE', #431, #17645 ) ;
#17132 = CARTESIAN_POINT ( 'NONE',  ( 2.682529543899157876, 8.255977015246598327, -7.033165578109189298 ) ) ;
#17133 = EDGE_CURVE ( 'NONE', #22463, #22670, #8226, .T. ) ;
#17134 = DIRECTION ( 'NONE',  ( -1.000000000000000000, -0.000000000000000000, -0.000000000000000000 ) ) ;
#17135 = ORIENTED_EDGE ( 'NONE', *, *, #22969, .T. ) ;
#17136 = CARTESIAN_POINT ( 'NONE',  ( 64.39795365981944997, 7.562528597612068045E-15, 0.000000000000000000 ) ) ;
#17137 = DIRECTION ( 'NONE',  ( -1.000000000000000000, -1.224606353822377258E-16, -0.000000000000000000 ) ) ;
#17138 = FACE_OUTER_BOUND ( 'NONE', #339, .T. ) ;
#17139 = DIRECTION ( 'NONE',  ( 0.000000000000000000, 0.000000000000000000, 1.000000000000000000 ) ) ;
#17140 = DIRECTION ( 'NONE',  ( 0.000000000000000000, 0.000000000000000000, 1.000000000000000000 ) ) ;
#17141 = DIRECTION ( 'NONE',  ( -1.000000000000000000, -0.000000000000000000, -0.000000000000000000 ) ) ;
#17142 = CARTESIAN_POINT ( 'NONE',  ( 64.39795365981944997, 7.562528597612068045E-15, 0.000000000000000000 ) ) ;
#17143 = AXIS2_PLACEMENT_3D ( 'NONE', #13037, #22110, #10840 ) ;
#17144 = EDGE_LOOP ( 'NONE', ( #7487, #10279, #17755, #3873, #7097, #10151 ) ) ;
#17145 = DIRECTION ( 'NONE',  ( -1.000000000000000000, 0.000000000000000000, 0.000000000000000000 ) ) ;
#17146 = PLANE ( 'NONE',  #9372 ) ;
#17147 = CARTESIAN_POINT ( 'NONE',  ( -29.00000000000000000, 29.49999999999999645, 12.00000000000000000 ) ) ;
#17148 = FACE_OUTER_BOUND ( 'NONE', #10093, .T. ) ;
#17149 = CARTESIAN_POINT ( 'NONE',  ( -5.365059087798940141, -7.384370330707086261, -11.93316557810918965 ) ) ;
#17150 = EDGE_CURVE ( 'NONE', #12632, #13595, #23186, .T. ) ;
#17151 = DIRECTION ( 'NONE',  ( -0.000000000000000000, -0.000000000000000000, 1.000000000000000000 ) ) ;
#17152 = ORIENTED_EDGE ( 'NONE', *, *, #6585, .T. ) ;
#17153 = ORIENTED_EDGE ( 'NONE', *, *, #14141, .F. ) ;
#17154 = EDGE_CURVE ( 'NONE', #8851, #9243, #1755, .T. ) ;
#17155 = CARTESIAN_POINT ( 'NONE',  ( 2.682529543900284974, -8.255977015246234174, 8.233165578109190363 ) ) ;
#17156 = ORIENTED_EDGE ( 'NONE', *, *, #6037, .F. ) ;
#17157 = DIRECTION ( 'NONE',  ( 0.9999997925849501978, 0.0006440730211826842938, 3.289528142814983993E-17 ) ) ;
#17158 =( BOUNDED_CURVE ( )  B_SPLINE_CURVE ( 2, ( #14783, #22244, #5516, #12949, #9645, #15615, #13443, #15383, #6128, #4559, #19065, #4302, #6369, #15758, #2224, #763, #395, #9888, #17091, #11704, #7802, #879, #9751, #18945, #11963, #19431, #13940, #19177, #6005, #2708, #2338, #10123, #21011, #8305, #17210, #15244, #17574, #23220, #21381, #2461, #22717, #8171, #13812, #20901, #6501, #11470, #4190, #6241, #11594, #10006, #517, #7933, #23082, #11842, #22853, #17345, #19311, #13569, #647, #8056, #15503, #22970, #13681, #21123, #21262, #4428, #2595, #17463, #10258, #18205, #14286, #14397, #12073, #17713, #12335, #8660, #14050, #8549, #21853, #10385, #1011, #21745, #1497, #12444, #19547, #16119, #19803, #21624, #21495, #6973, #20032, #5034, #8435, #15883, #4923, #14167, #23582 ),
 .UNSPECIFIED., .F., .F. ) 
 B_SPLINE_CURVE_WITH_KNOTS ( ( 3, 2, 2, 2, 2, 2, 2, 2, 2, 2, 2, 2, 2, 2, 2, 2, 2, 2, 2, 2, 2, 2, 2, 2, 2, 2, 2, 2, 2, 2, 2, 2, 2, 2, 2, 2, 2, 2, 2, 2, 2, 2, 2, 2, 2, 2, 2, 2, 3 ),
 ( 0.01324393663734861268, 0.02000000000000000042, 0.04000000000000000083, 0.05999999999999999778, 0.07999999999999998779, 0.1000000000000000056, 0.1199999999999999956, 0.1400000000000000133, 0.1600000000000000033, 0.1799999999999999933, 0.2000000000000000111, 0.2200000000000000011, 0.2399999999999999911, 0.2600000000000000089, 0.2800000000000000266, 0.2999999999999999889, 0.3200000000000000067, 0.3400000000000000244, 0.3599999999999999867, 0.3800000000000000044, 0.4000000000000000222, 0.4199999999999999845, 0.4400000000000000022, 0.4600000000000000200, 0.4799999999999999822, 0.5000000000000000000, 0.5200000000000000178, 0.5400000000000000355, 0.5600000000000000533, 0.5799999999999999600, 0.5999999999999999778, 0.6199999999999999956, 0.6400000000000000133, 0.6600000000000000311, 0.6800000000000000488, 0.6999999999999999556, 0.7199999999999999734, 0.7399999999999998801, 0.7600000000000000089, 0.7800000000000000266, 0.8000000000000000444, 0.8199999999999999512, 0.8399999999999999689, 0.8599999999999999867, 0.8800000000000000044, 0.9000000000000000222, 0.9200000000000000400, 0.9399999999999999467, 0.9500000000000000666 ),
 .UNSPECIFIED. ) 
 CURVE ( )  GEOMETRIC_REPRESENTATION_ITEM ( )  RATIONAL_B_SPLINE_CURVE ( ( 0.9781034501096583789, 0.9834667361450580847, 1.000000000000000000, 0.9510565162951535312, 1.000000000000000000, 0.9510565162951535312, 1.000000000000000000, 0.9510565162951535312, 1.000000000000000000, 0.9510565162951535312, 1.000000000000000000, 0.9510565162951535312, 1.000000000000000000, 0.9510565162951535312, 1.000000000000000000, 0.9510565162951535312, 1.000000000000000000, 0.9510565162951535312, 1.000000000000000000, 0.9510565162951535312, 1.000000000000000000, 0.9510565162951535312, 1.000000000000000000, 0.9510565162951535312, 1.000000000000000000, 0.9510565162951535312, 1.000000000000000000, 0.9510565162951535312, 1.000000000000000000, 0.9510565162951535312, 1.000000000000000000, 0.9510565162951535312, 1.000000000000000000, 0.9510565162951535312, 1.000000000000000000, 0.9510565162951535312, 1.000000000000000000, 0.9510565162951535312, 1.000000000000000000, 0.9510565162951535312, 1.000000000000000000, 0.9510565162951535312, 1.000000000000000000, 0.9510565162951535312, 1.000000000000000000, 0.9510565162951535312, 1.000000000000000000, 0.9510565162951535312, 1.000000000000000000, 0.9510565162951535312, 1.000000000000000000, 0.9510565162951535312, 1.000000000000000000, 0.9510565162951535312, 1.000000000000000000, 0.9510565162951535312, 1.000000000000000000, 0.9510565162951535312, 1.000000000000000000, 0.9510565162951535312, 1.000000000000000000, 0.9510565162951535312, 1.000000000000000000, 0.9510565162951535312, 1.000000000000000000, 0.9510565162951535312, 1.000000000000000000, 0.9510565162951535312, 1.000000000000000000, 0.9510565162951535312, 1.000000000000000000, 0.9510565162951535312, 1.000000000000000000, 0.9510565162951535312, 1.000000000000000000, 0.9510565162951535312, 1.000000000000000000, 0.9510565162951535312, 1.000000000000000000, 0.9510565162951535312, 1.000000000000000000, 0.9510565162951535312, 1.000000000000000000, 0.9510565162951535312, 1.000000000000000000, 0.9510565162951535312, 1.000000000000000000, 0.9510565162951535312, 1.000000000000000000, 0.9510565162951535312, 1.000000000000000000, 0.9510565162951535312, 1.000000000000000000, 0.9510565162951535312, 1.000000000000000000, 0.9755282581475764880, 0.9755282581475768211 ) ) 
 REPRESENTATION_ITEM ( '' )  );
#17159 = LINE ( 'NONE', #14843, #17915 ) ;
#17160 = AXIS2_PLACEMENT_3D ( 'NONE', #21261, #6126, #22852 ) ;
#17161 = ORIENTED_EDGE ( 'NONE', *, *, #20141, .F. ) ;
#17162 = CARTESIAN_POINT ( 'NONE',  ( 2.570122167802765922, 0.000000000000000000, 0.000000000000000000 ) ) ;
#17163 = CARTESIAN_POINT ( 'NONE',  ( 40.23082370883260239, 29.49999999999999645, -3.000000000000000000 ) ) ;
#17164 = CARTESIAN_POINT ( 'NONE',  ( 66.14750088563508257, -9.244463733058732095E-30, 5.000000000000007994 ) ) ;
#17165 = CARTESIAN_POINT ( 'NONE',  ( -42.00000000000000000, 6.000000000000000888, 12.00000000000000000 ) ) ;
#17166 = ORIENTED_EDGE ( 'NONE', *, *, #6502, .T. ) ;
#17167 = ADVANCED_BREP_SHAPE_REPRESENTATION ( '', ( #10155, #8005 ), #20496 ) ;
#17168 = DIRECTION ( 'NONE',  ( 0.000000000000000000, 0.000000000000000000, -1.000000000000000000 ) ) ;
#17169 = CARTESIAN_POINT ( 'NONE',  ( -41.58578643762692195, -26.57671364288190574, 12.00000000000000355 ) ) ;
#17170 = EDGE_LOOP ( 'NONE', ( #16855, #20572, #3514, #2577, #7475 ) ) ;
#17171 = DIRECTION ( 'NONE',  ( -1.000000000000000000, 0.000000000000000000, 0.000000000000000000 ) ) ;
#17172 = DIRECTION ( 'NONE',  ( 0.000000000000000000, -1.000000000000000000, 0.000000000000000000 ) ) ;
#17173 = CARTESIAN_POINT ( 'NONE',  ( -9.499999999999790390, -3.086737114213257804, 4.306742014460233747 ) ) ;
#17174 = ORIENTED_EDGE ( 'NONE', *, *, #6648, .T. ) ;
#17175 =( GEOMETRIC_REPRESENTATION_CONTEXT ( 3 ) GLOBAL_UNCERTAINTY_ASSIGNED_CONTEXT ( ( #21335 ) ) GLOBAL_UNIT_ASSIGNED_CONTEXT ( ( #15070, #5814, #9584 ) ) REPRESENTATION_CONTEXT ( 'NONE', 'WORKASPACE' ) );
#17176 = DIRECTION ( 'NONE',  ( -0.000000000000000000, -0.000000000000000000, -1.000000000000000000 ) ) ;
#17177 = ORIENTED_EDGE ( 'NONE', *, *, #5462, .T. ) ;
#17178 = ORIENTED_EDGE ( 'NONE', *, *, #11273, .F. ) ;
#17179 = CARTESIAN_POINT ( 'NONE',  ( 5.871322893123449127, 8.081182679344781405, 8.359589141758144493 ) ) ;
#17180 = EDGE_CURVE ( 'NONE', #6887, #21201, #8597, .T. ) ;
#17181 = ADVANCED_FACE ( 'NONE', ( #9944 ), #14098, .T. ) ;
#17182 = ORIENTED_EDGE ( 'NONE', *, *, #7021, .F. ) ;
#17183 =( NAMED_UNIT ( * ) PLANE_ANGLE_UNIT ( ) SI_UNIT ( $, .RADIAN. ) );
#17184 = DIRECTION ( 'NONE',  ( -1.000000000000000000, 0.000000000000000000, 0.000000000000000000 ) ) ;
#17185 = DIRECTION ( 'NONE',  ( 0.000000000000000000, 0.000000000000000000, 1.000000000000000000 ) ) ;
#17186 = DIRECTION ( 'NONE',  ( 0.000000000000000000, 0.000000000000000000, 1.000000000000000000 ) ) ;
#17187 = DIRECTION ( 'NONE',  ( -1.000000000000000000, 0.000000000000000000, 0.000000000000000000 ) ) ;
#17188 = VECTOR ( 'NONE', #18231, 1000.000000000000000 ) ;
#17189 = CARTESIAN_POINT ( 'NONE',  ( 31.10231664966676846, 45.36128193761570770, 11.00000000000000000 ) ) ;
#17190 = CARTESIAN_POINT ( 'NONE',  ( 0.000000000000000000, 0.000000000000000000, 105.0000000000000000 ) ) ;
#17191 = AXIS2_PLACEMENT_3D ( 'NONE', #10049, #8214, #4226 ) ;
#17192 = CIRCLE ( 'NONE', #10578, 5.000000000000007994 ) ;
#17193 = CARTESIAN_POINT ( 'NONE',  ( 9.000000000000000000, 0.000000000000000000, 0.9999999999999731326 ) ) ;
#17194 = ORIENTED_EDGE ( 'NONE', *, *, #3735, .F. ) ;
#17195 = CARTESIAN_POINT ( 'NONE',  ( 41.00000000000000000, 4.999999999999986677, 11.00000000000000000 ) ) ;
#17196 = ORIENTED_EDGE ( 'NONE', *, *, #16266, .F. ) ;
#17197 = CARTESIAN_POINT ( 'NONE',  ( 2.500152530714462085, -8.687388223084449024, 12.46832088299141716 ) ) ;
#17198 = CARTESIAN_POINT ( 'NONE',  ( 67.60204634018053582, 7.420530141404717394E-15, 0.000000000000000000 ) ) ;
#17199 = EDGE_CURVE ( 'NONE', #20548, #14991, #15370, .T. ) ;
#17200 = DIRECTION ( 'NONE',  ( -1.000000000000000000, 0.000000000000000000, 0.000000000000000000 ) ) ;
#17201 = DIRECTION ( 'NONE',  ( 1.000000000000000000, 0.000000000000000000, 0.000000000000000000 ) ) ;
#17202 = DIRECTION ( 'NONE',  ( 0.000000000000000000, 0.000000000000000000, -1.000000000000000000 ) ) ;
#17203 = DIRECTION ( 'NONE',  ( -1.000000000000000000, 0.000000000000000000, 0.000000000000000000 ) ) ;
#17204 = ADVANCED_FACE ( 'NONE', ( #2758 ), #8491, .F. ) ;
#17205 = CARTESIAN_POINT ( 'NONE',  ( -5.871322893124554021, 8.081182679343978492, -5.906742014460233392 ) ) ;
#17206 = AXIS2_PLACEMENT_3D ( 'NONE', #8515, #10460, #14125 ) ;
#17207 = ORIENTED_EDGE ( 'NONE', *, *, #16699, .F. ) ;
#17208 = VECTOR ( 'NONE', #4541, 1000.000000000000000 ) ;
#17209 = DIRECTION ( 'NONE',  ( 1.000000000000000000, 0.000000000000000000, 0.000000000000000000 ) ) ;
#17210 = CARTESIAN_POINT ( 'NONE',  ( -2.682529543900285862, 8.255977015246234174, 9.233165578109188587 ) ) ;
#17211 = EDGE_CURVE ( 'NONE', #11604, #23403, #10425, .T. ) ;
#17212 = VECTOR ( 'NONE', #19052, 1000.000000000000000 ) ;
#17213 = ADVANCED_FACE ( 'NONE', ( #12130 ), #19607, .F. ) ;
#17214 = EDGE_CURVE ( 'NONE', #758, #22790, #17778, .T. ) ;
#17215 = AXIS2_PLACEMENT_3D ( 'NONE', #6222, #9866, #11946 ) ;
#17216 = DIRECTION ( 'NONE',  ( 1.000000000000000000, 0.000000000000000000, -0.000000000000000000 ) ) ;
#17217 = CARTESIAN_POINT ( 'NONE',  ( -41.99999999999999289, 0.000000000000000000, 0.000000000000000000 ) ) ;
#17218 = ORIENTED_EDGE ( 'NONE', *, *, #19719, .F. ) ;
#17219 = ORIENTED_EDGE ( 'NONE', *, *, #21052, .T. ) ;
#17220 = ORIENTED_EDGE ( 'NONE', *, *, #20097, .T. ) ;
#17221 = CARTESIAN_POINT ( 'NONE',  ( 41.99999999999999289, 5.618459588085056979E-15, 0.000000000000000000 ) ) ;
#17222 = CARTESIAN_POINT ( 'NONE',  ( 9.499999999999790390, 3.086737114213260025, -9.306742014460233747 ) ) ;
#17223 = VERTEX_POINT ( 'NONE', #4356 ) ;
#17224 = AXIS2_PLACEMENT_3D ( 'NONE', #22186, #20115, #23768 ) ;
#17225 = TOROIDAL_SURFACE ( 'NONE', #18410, 6.500000000000000888, 1.500000000000000000 ) ;
#17226 = CIRCLE ( 'NONE', #20359, 14.99999999999999822 ) ;
#17227 = FACE_BOUND ( 'NONE', #6375, .T. ) ;
#17228 = VECTOR ( 'NONE', #16696, 1000.000000000000000 ) ;
#17229 = ORIENTED_EDGE ( 'NONE', *, *, #10741, .T. ) ;
#17230 = CARTESIAN_POINT ( 'NONE',  ( 35.99999999999999289, -51.00000000000000711, 0.5000000000000000000 ) ) ;
#17231 = AXIS2_PLACEMENT_3D ( 'NONE', #15495, #6121, #20895 ) ;
#17232 = ADVANCED_FACE ( 'NONE', ( #13620 ), #23151, .T. ) ;
#17233 = ORIENTED_EDGE ( 'NONE', *, *, #22227, .T. ) ;
#17234 = DIRECTION ( 'NONE',  ( -0.000000000000000000, -0.000000000000000000, -1.000000000000000000 ) ) ;
#17235 = TOROIDAL_SURFACE ( 'NONE', #10234, 10.49999999999999822, 1.000000000000000000 ) ;
#17236 = FACE_OUTER_BOUND ( 'NONE', #22273, .T. ) ;
#17237 = DIRECTION ( 'NONE',  ( -0.000000000000000000, -0.000000000000000000, -1.000000000000000000 ) ) ;
#17238 = CARTESIAN_POINT ( 'NONE',  ( 43.50000000000000711, 25.84341543330623026, 0.000000000000000000 ) ) ;
#17239 = EDGE_LOOP ( 'NONE', ( #2371, #12958, #10611, #16739 ) ) ;
#17240 = DIRECTION ( 'NONE',  ( 0.000000000000000000, -1.000000000000000000, 0.000000000000000000 ) ) ;
#17241 = FACE_OUTER_BOUND ( 'NONE', #18080, .T. ) ;
#17242 = ADVANCED_FACE ( 'NONE', ( #21060, #8109 ), #11763, .T. ) ;
#17243 = ORIENTED_EDGE ( 'NONE', *, *, #16647, .F. ) ;
#17244 = EDGE_CURVE ( 'NONE', #14989, #16538, #4048, .T. ) ;
#17245 = ORIENTED_EDGE ( 'NONE', *, *, #9077, .T. ) ;
#17246 = CARTESIAN_POINT ( 'NONE',  ( 7.022953521755574080, -5.102474405759714671, 6.433165578109188765 ) ) ;
#17247 = ORIENTED_EDGE ( 'NONE', *, *, #3669, .T. ) ;
#17248 = VECTOR ( 'NONE', #3141, 1000.000000000000000 ) ;
#17249 = AXIS2_PLACEMENT_3D ( 'NONE', #17947, #20257, #6848 ) ;
#17250 = ORIENTED_EDGE ( 'NONE', *, *, #16741, .T. ) ;
#17251 = AXIS2_PLACEMENT_3D ( 'NONE', #5178, #12734, #21666 ) ;
#17252 = CARTESIAN_POINT ( 'NONE',  ( 2.935661446562616295, -9.035036904803758873, 5.659589141758144315 ) ) ;
#17253 = CIRCLE ( 'NONE', #21564, 14.02592346138681201 ) ;
#17254 = ORIENTED_EDGE ( 'NONE', *, *, #16875, .T. ) ;
#17255 = ORIENTED_EDGE ( 'NONE', *, *, #14221, .F. ) ;
#17256 = DIRECTION ( 'NONE',  ( -1.000000000000000000, 0.000000000000000000, 0.000000000000000000 ) ) ;
#17257 = CARTESIAN_POINT ( 'NONE',  ( 41.50000000000000000, -28.80990663662250739, 12.00000000000000000 ) ) ;
#17258 = CONICAL_SURFACE ( 'NONE', #12951, 4.172000000000008590, 0.9599310885968742602 ) ;
#17259 = ORIENTED_EDGE ( 'NONE', *, *, #992, .F. ) ;
#17260 = DIRECTION ( 'NONE',  ( -1.000000000000000000, 0.000000000000000000, 0.000000000000000000 ) ) ;
#17261 = DIRECTION ( 'NONE',  ( -1.000000000000000000, -1.224606353822377258E-16, -0.000000000000000000 ) ) ;
#17262 = DIRECTION ( 'NONE',  ( -1.000000000000000000, -1.224606353822377258E-16, -0.000000000000000000 ) ) ;
#17263 = DIRECTION ( 'NONE',  ( -0.000000000000000000, -0.000000000000000000, -1.000000000000000000 ) ) ;
#17264 = ORIENTED_EDGE ( 'NONE', *, *, #23956, .F. ) ;
#17265 = CARTESIAN_POINT ( 'NONE',  ( 89.17200000000002547, 6.123233995736768255E-16, -5.000000000000000888 ) ) ;
#17266 = DIRECTION ( 'NONE',  ( 0.000000000000000000, -1.000000000000000000, 0.000000000000000000 ) ) ;
#17267 = AXIS2_PLACEMENT_3D ( 'NONE', #5760, #21790, #7679 ) ;
#17268 = VECTOR ( 'NONE', #333, 999.9999999999998863 ) ;
#17269 = EDGE_LOOP ( 'NONE', ( #19198, #12863 ) ) ;
#17270 = FACE_OUTER_BOUND ( 'NONE', #9529, .T. ) ;
#17271 = DIRECTION ( 'NONE',  ( 4.613626265895764052E-16, 1.000000000000000000, 0.000000000000000000 ) ) ;
#17272 = AXIS2_PLACEMENT_3D ( 'NONE', #11864, #14184, #6755 ) ;
#17273 = LINE ( 'NONE', #18874, #9121 ) ;
#17274 = AXIS2_PLACEMENT_3D ( 'NONE', #17980, #1269, #12467 ) ;
#17275 = DIRECTION ( 'NONE',  ( -1.000000000000000000, -0.000000000000000000, -0.000000000000000000 ) ) ;
#17276 = AXIS2_PLACEMENT_3D ( 'NONE', #12744, #20205, #10894 ) ;
#17277 = CARTESIAN_POINT ( 'NONE',  ( -8.680847955711007202, -5.923547351154968927E-13, -9.633165578109188942 ) ) ;
#17278 = EDGE_CURVE ( 'NONE', #4776, #3225, #2888, .T. ) ;
#17279 = CIRCLE ( 'NONE', #23132, 5.000000000000007994 ) ;
#17280 = EDGE_LOOP ( 'NONE', ( #2167, #9185, #2484, #1102 ) ) ;
#17281 = ORIENTED_EDGE ( 'NONE', *, *, #21264, .F. ) ;
#17282 = CARTESIAN_POINT ( 'NONE',  ( -8.680847955711007202, -5.923547351154968927E-13, 9.633165578109188942 ) ) ;
#17283 = VERTEX_POINT ( 'NONE', #8846 ) ;
#17284 = CARTESIAN_POINT ( 'NONE',  ( -6.822232771736904647E-13, 9.988891130263535700, -11.70674201446023410 ) ) ;
#17285 = ORIENTED_EDGE ( 'NONE', *, *, #5248, .T. ) ;
#17286 = CYLINDRICAL_SURFACE ( 'NONE', #16931, 5.000000000000000888 ) ;
#17287 = CARTESIAN_POINT ( 'NONE',  ( -28.27483331787888687, 41.23752903419610050, 11.00000000000000000 ) ) ;
#17288 = AXIS2_PLACEMENT_3D ( 'NONE', #7440, #22366, #20761 ) ;
#17289 = AXIS2_PLACEMENT_3D ( 'NONE', #5696, #6051, #9793 ) ;
#17290 = CARTESIAN_POINT ( 'NONE',  ( 4.810877257134742457, -7.548248927254282314, 12.50000000000000000 ) ) ;
#17291 = DIRECTION ( 'NONE',  ( -0.000000000000000000, -0.000000000000000000, 1.000000000000000000 ) ) ;
#17292 = DIRECTION ( 'NONE',  ( 1.000000000000000000, 0.000000000000000000, 0.000000000000000000 ) ) ;
#17293 = ORIENTED_EDGE ( 'NONE', *, *, #24009, .F. ) ;
#17294 = AXIS2_PLACEMENT_3D ( 'NONE', #13964, #21409, #4694 ) ;
#17295 = EDGE_CURVE ( 'NONE', #4703, #8138, #8953, .T. ) ;
#17296 = VECTOR ( 'NONE', #20578, 1000.000000000000000 ) ;
#17297 = ORIENTED_EDGE ( 'NONE', *, *, #3612, .T. ) ;
#17298 = DIRECTION ( 'NONE',  ( 0.000000000000000000, 1.000000000000000000, 0.000000000000000000 ) ) ;
#17299 = DIRECTION ( 'NONE',  ( 0.000000000000000000, -1.000000000000000000, 0.000000000000000000 ) ) ;
#17300 = VECTOR ( 'NONE', #11301, 1000.000000000000000 ) ;
#17301 = EDGE_CURVE ( 'NONE', #21814, #20489, #2479, .T. ) ;
#17302 = DIRECTION ( 'NONE',  ( -0.000000000000000000, -0.000000000000000000, -1.000000000000000000 ) ) ;
#17303 = CARTESIAN_POINT ( 'NONE',  ( -31.74999999999995737, 0.000000000000000000, 0.000000000000000000 ) ) ;
#17304 = CARTESIAN_POINT ( 'NONE',  ( -29.00000000000000000, 29.49999999999999645, 11.50000000000000000 ) ) ;
#17305 = CARTESIAN_POINT ( 'NONE',  ( 8.000000000000000000, 0.000000000000000000, -12.50000000000000000 ) ) ;
#17306 = EDGE_CURVE ( 'NONE', #19937, #20363, #17687, .T. ) ;
#17307 = B_SPLINE_CURVE_WITH_KNOTS ( 'NONE', 3,
 ( #4415, #11827, #2083, #22486, #5762, #9637, #13177, #20635 ),
 .UNSPECIFIED., .F., .F.,
 ( 4, 2, 2, 4 ),
 ( 4.336808689942017736E-19, 0.001946159586596638924, 0.002919239379894958061, 0.003892319173193277415 ),
 .UNSPECIFIED. ) ;
#17308 = CARTESIAN_POINT ( 'NONE',  ( 9.500000000000000000, 6.470877716354879437E-13, 5.206742014460234103 ) ) ;
#17309 = ORIENTED_EDGE ( 'NONE', *, *, #13419, .F. ) ;
#17310 = CARTESIAN_POINT ( 'NONE',  ( 8.680847955711007202, 5.912916378492122225E-13, -6.633165578109188942 ) ) ;
#17311 = EDGE_LOOP ( 'NONE', ( #1034, #18743, #20100, #4984 ) ) ;
#17312 = AXIS2_PLACEMENT_3D ( 'NONE', #11706, #4563, #19313 ) ;
#17313 = ORIENTED_EDGE ( 'NONE', *, *, #6379, .F. ) ;
#17314 = CARTESIAN_POINT ( 'NONE',  ( 5.871322893124553133, -8.081182679343980269, 11.75958914175814485 ) ) ;
#17315 = CARTESIAN_POINT ( 'NONE',  ( -23.85000000000000142, -15.03999999999999737, 2.200000000000000178 ) ) ;
#17316 = ORIENTED_EDGE ( 'NONE', *, *, #2447, .F. ) ;
#17317 = DIRECTION ( 'NONE',  ( -1.000000000000000000, -1.224606353822377258E-16, -0.000000000000000000 ) ) ;
#17318 = AXIS2_PLACEMENT_3D ( 'NONE', #8759, #21586, #2667 ) ;
#17319 = CARTESIAN_POINT ( 'NONE',  ( -44.00000000000000711, -51.00000000000000711, 0.5000000000000000000 ) ) ;
#17320 = FACE_OUTER_BOUND ( 'NONE', #23168, .T. ) ;
#17321 = CARTESIAN_POINT ( 'NONE',  ( 3.934052222107162766, -8.094642247421043990, -12.50000000000000000 ) ) ;
#17322 = DIRECTION ( 'NONE',  ( -0.000000000000000000, -0.000000000000000000, -1.000000000000000000 ) ) ;
#17323 = CIRCLE ( 'NONE', #16542, 5.099999999999996980 ) ;
#17324 = CARTESIAN_POINT ( 'NONE',  ( -6.153822176767817416E-13, 9.500000000000000000, -2.559589141758142450 ) ) ;
#17325 = ORIENTED_EDGE ( 'NONE', *, *, #23461, .T. ) ;
#17326 = VECTOR ( 'NONE', #13, 1000.000000000000000 ) ;
#17327 = DIRECTION ( 'NONE',  ( 0.8571673007021116675, 1.049727191138617833E-16, -0.5150380749100552658 ) ) ;
#17328 = EDGE_CURVE ( 'NONE', #10172, #8836, #3364, .T. ) ;
#17329 = ADVANCED_FACE ( 'NONE', ( #1775 ), #3478, .T. ) ;
#17330 = ORIENTED_EDGE ( 'NONE', *, *, #4003, .T. ) ;
#17331 = FACE_OUTER_BOUND ( 'NONE', #5120, .T. ) ;
#17332 = DIRECTION ( 'NONE',  ( -0.000000000000000000, -0.000000000000000000, -1.000000000000000000 ) ) ;
#17333 = SURFACE_SIDE_STYLE ('',( #11459 ) ) ;
#17334 = VECTOR ( 'NONE', #10722, 1000.000000000000000 ) ;
#17335 = CARTESIAN_POINT ( 'NONE',  ( -36.00000000000001421, 50.99999999999999289, 0.5000000000000000000 ) ) ;
#17336 = DIRECTION ( 'NONE',  ( 0.000000000000000000, 0.000000000000000000, 1.000000000000000000 ) ) ;
#17337 = FACE_OUTER_BOUND ( 'NONE', #4566, .T. ) ;
#17338 = CARTESIAN_POINT ( 'NONE',  ( 24.75000000000000711, -29.50000000000000000, -3.000000000000000000 ) ) ;
#17339 = CONICAL_SURFACE ( 'NONE', #18898, 2.024999999999999911, 0.7853981633974743692 ) ;
#17340 = CIRCLE ( 'NONE', #4900, 5.000000000000007994 ) ;
#17341 = EDGE_LOOP ( 'NONE', ( #5690, #13839, #13239, #14678 ) ) ;
#17342 = CARTESIAN_POINT ( 'NONE',  ( 23.00000000000000000, 0.000000000000000000, 0.000000000000000000 ) ) ;
#17343 = ORIENTED_EDGE ( 'NONE', *, *, #23666, .T. ) ;
#17344 = PLANE ( 'NONE',  #17949 ) ;
#17345 = CARTESIAN_POINT ( 'NONE',  ( -6.233975306307045953E-13, 9.127583699786111282, 7.133165578109187166 ) ) ;
#17346 = DIRECTION ( 'NONE',  ( -0.000000000000000000, -0.000000000000000000, -1.000000000000000000 ) ) ;
#17347 = DIRECTION ( 'NONE',  ( -1.000000000000000000, 0.000000000000000000, 0.000000000000000000 ) ) ;
#17348 = DIRECTION ( 'NONE',  ( 0.000000000000000000, 0.000000000000000000, 1.000000000000000000 ) ) ;
#17349 = PRODUCT_DEFINITION ( 'UNKNOWN', '', #21688, #23109 ) ;
#17350 = EDGE_CURVE ( 'NONE', #10011, #18514, #23640, .T. ) ;
#17351 = AXIS2_PLACEMENT_3D ( 'NONE', #3319, #12566, #23589 ) ;
#17352 = VERTEX_POINT ( 'NONE', #23507 ) ;
#17353 = DIRECTION ( 'NONE',  ( -1.000000000000000000, 0.000000000000000000, 0.000000000000000000 ) ) ;
#17354 = AXIS2_PLACEMENT_3D ( 'NONE', #13991, #6432, #15933 ) ;
#17355 = EDGE_CURVE ( 'NONE', #3765, #8089, #942, .T. ) ;
#17356 = VECTOR ( 'NONE', #871, 1000.000000000000000 ) ;
#17357 = CARTESIAN_POINT ( 'NONE',  ( -7.685661446561619314, -5.583959896779019161, -8.406742014460233392 ) ) ;
#17358 = VERTEX_POINT ( 'NONE', #20313 ) ;
#17359 = ORIENTED_EDGE ( 'NONE', *, *, #23732, .F. ) ;
#17360 = EDGE_CURVE ( 'NONE', #20283, #15320, #20806, .T. ) ;
#17361 = EDGE_CURVE ( 'NONE', #10579, #21873, #19657, .T. ) ;
#17362 = PLANE ( 'NONE',  #5091 ) ;
#17363 = ORIENTED_EDGE ( 'NONE', *, *, #20845, .F. ) ;
#17364 = ORIENTED_EDGE ( 'NONE', *, *, #14718, .F. ) ;
#17365 = CIRCLE ( 'NONE', #19334, 9.999999999999998224 ) ;
#17366 = DIRECTION ( 'NONE',  ( -1.000000000000000000, -1.224606353822377258E-16, -0.000000000000000000 ) ) ;
#17367 = FACE_OUTER_BOUND ( 'NONE', #14648, .T. ) ;
#17368 = CARTESIAN_POINT ( 'NONE',  ( -34.00000000000000000, -4.999999999999999112, 9.500000000000000000 ) ) ;
#17369 = AXIS2_PLACEMENT_3D ( 'NONE', #20603, #13141, #3639 ) ;
#17370 = DIRECTION ( 'NONE',  ( -0.000000000000000000, -0.000000000000000000, -1.000000000000000000 ) ) ;
#17371 = ORIENTED_EDGE ( 'NONE', *, *, #22302, .T. ) ;
#17372 = CARTESIAN_POINT ( 'NONE',  ( -34.10000000000000142, 29.49999999999999645, 11.50000000000000000 ) ) ;
#17373 = DIRECTION ( 'NONE',  ( 0.5735764363510424957, 0.8191520442889943521, 0.000000000000000000 ) ) ;
#17374 = CARTESIAN_POINT ( 'NONE',  ( 23.00000000000000000, 0.000000000000000000, 0.000000000000000000 ) ) ;
#17375 = ORIENTED_EDGE ( 'NONE', *, *, #5668, .T. ) ;
#17376 = AXIS2_PLACEMENT_3D ( 'NONE', #24082, #20424, #12613 ) ;
#17377 = B_SPLINE_CURVE_WITH_KNOTS ( 'NONE', 3,
 ( #7891, #2184, #17057, #15341, #20613, #22812, #357, #2056, #6091, #18663, #7769, #252, #20370, #1833, #9480, #7411, #22329, #22455, #5611, #13033, #20494, #1937, #9352, #16938, #124, #5735, #3891, #18769, #7658, #23046, #22933, #6208, #21218, #4523, #20976, #10344 ),
 .UNSPECIFIED., .F., .F.,
 ( 4, 2, 2, 2, 2, 2, 2, 2, 2, 2, 2, 2, 2, 2, 2, 2, 2, 4 ),
 ( 4.249187360970369464E-18, 0.002901772246161924990, 0.003627215307702405262, 0.004352658369242885100, 0.005803544492323838705, 0.006528987553864317242, 0.007254430615404792310, 0.008705316738485749384, 0.01015620286156670646, 0.01160708898464766527, 0.01305797510772862408, 0.01450886123080957942, 0.01595974735389053822, 0.01741063347697149530, 0.01886151960005245584, 0.02031240572313341639, 0.02176329184621437693, 0.02321417796929533747 ),
 .UNSPECIFIED. ) ;
#17378 = CONICAL_SURFACE ( 'NONE', #15008, 4.249999999999996447, 1.029744258676654090 ) ;
#17379 = VERTEX_POINT ( 'NONE', #14218 ) ;
#17380 = CARTESIAN_POINT ( 'NONE',  ( -5.871322893123450015, -8.081182679344781405, 7.359589141758143604 ) ) ;
#17381 = EDGE_LOOP ( 'NONE', ( #13686, #21588, #17153 ) ) ;
#17382 = VERTEX_POINT ( 'NONE', #22160 ) ;
#17383 = ORIENTED_EDGE ( 'NONE', *, *, #12616, .F. ) ;
#17384 = EDGE_CURVE ( 'NONE', #5799, #5565, #1329, .T. ) ;
#17385 = ORIENTED_EDGE ( 'NONE', *, *, #21675, .F. ) ;
#17386 = VERTEX_POINT ( 'NONE', #10543 ) ;
#17387 = ORIENTED_EDGE ( 'NONE', *, *, #16218, .F. ) ;
#17388 = CARTESIAN_POINT ( 'NONE',  ( 23.00000000000000000, -17.86986844953242226, -0.4282833139928861610 ) ) ;
#17389 = CARTESIAN_POINT ( 'NONE',  ( 7.022953521754877748, 5.102474405760673903, -4.833165578109188232 ) ) ;
#17390 = CARTESIAN_POINT ( 'NONE',  ( -14.91530227160598621, -1.623290104782665999, -9.365835742197237579 ) ) ;
#17391 = CIRCLE ( 'NONE', #16997, 2.500000000000002220 ) ;
#17392 = ORIENTED_EDGE ( 'NONE', *, *, #21970, .T. ) ;
#17393 = CARTESIAN_POINT ( 'NONE',  ( -31.10231664966676135, 45.36128193761570770, 27.00000000000000000 ) ) ;
#17394 = DIRECTION ( 'NONE',  ( 1.000000000000000000, 1.224606353822377258E-16, 0.000000000000000000 ) ) ;
#17395 = DIRECTION ( 'NONE',  ( -1.000000000000000000, -0.000000000000000000, -0.000000000000000000 ) ) ;
#17396 = EDGE_CURVE ( 'NONE', #12189, #19800, #8725, .T. ) ;
#17397 = EDGE_CURVE ( 'NONE', #8229, #16379, #3324, .T. ) ;
#17398 = DIRECTION ( 'NONE',  ( -1.000000000000000000, 0.000000000000000000, 0.000000000000000000 ) ) ;
#17399 = ORIENTED_EDGE ( 'NONE', *, *, #18153, .F. ) ;
#17400 = CIRCLE ( 'NONE', #9596, 1.499999999999994449 ) ;
#17401 = DIRECTION ( 'NONE',  ( 0.000000000000000000, -1.000000000000000000, 0.000000000000000000 ) ) ;
#17402 = ORIENTED_EDGE ( 'NONE', *, *, #19300, .F. ) ;
#17403 = CARTESIAN_POINT ( 'NONE',  ( -31.74999999999995737, 6.123233995736767268E-16, -5.000000000000000888 ) ) ;
#17404 = LINE ( 'NONE', #22779, #14457 ) ;
#17405 = CARTESIAN_POINT ( 'NONE',  ( 5.000000000000000000, 0.000000000000000000, 0.000000000000000000 ) ) ;
#17406 = CARTESIAN_POINT ( 'NONE',  ( -8.680847955710813579, -2.820578480814257549, -5.733165578109188587 ) ) ;
#17407 = CIRCLE ( 'NONE', #4960, 5.000000000000007994 ) ;
#17408 = ORIENTED_EDGE ( 'NONE', *, *, #21007, .F. ) ;
#17409 = DIRECTION ( 'NONE',  ( -1.000000000000000000, 0.000000000000000000, 0.000000000000000000 ) ) ;
#17410 = ORIENTED_EDGE ( 'NONE', *, *, #16363, .T. ) ;
#17411 = ORIENTED_EDGE ( 'NONE', *, *, #23341, .T. ) ;
#17412 = CARTESIAN_POINT ( 'NONE',  ( -5.365059087799947335, 7.384370330706355290, -11.33316557810918468 ) ) ;
#17413 = CARTESIAN_POINT ( 'NONE',  ( 2.682529543900284974, -8.255977015246234174, 10.23316557810918859 ) ) ;
#17414 = VERTEX_POINT ( 'NONE', #5321 ) ;
#17415 = CARTESIAN_POINT ( 'NONE',  ( 1359.670837123689580, 1745.668304299772444, 10.22831690717758768 ) ) ;
#17416 = VERTEX_POINT ( 'NONE', #18250 ) ;
#17417 = DIRECTION ( 'NONE',  ( -0.000000000000000000, -0.000000000000000000, 1.000000000000000000 ) ) ;
#17418 = CARTESIAN_POINT ( 'NONE',  ( 9.499999999999790390, 3.086737114213260025, -10.15958914175814520 ) ) ;
#17419 = CARTESIAN_POINT ( 'NONE',  ( 0.000000000000000000, -2.342598717236916261, -4.057499999999997442 ) ) ;
#17420 = CARTESIAN_POINT ( 'NONE',  ( -39.00000000000000711, -29.49999999999999645, 12.00000000000000000 ) ) ;
#17421 = CARTESIAN_POINT ( 'NONE',  ( 0.000000000000000000, 0.000000000000000000, 0.000000000000000000 ) ) ;
#17422 = EDGE_CURVE ( 'NONE', #10822, #17524, #22756, .T. ) ;
#17423 = DIRECTION ( 'NONE',  ( -0.000000000000000000, 0.000000000000000000, 1.000000000000000000 ) ) ;
#17424 = EDGE_CURVE ( 'NONE', #17662, #9768, #20087, .T. ) ;
#17425 = DIRECTION ( 'NONE',  ( 0.000000000000000000, 0.000000000000000000, 1.000000000000000000 ) ) ;
#17426 = DIRECTION ( 'NONE',  ( -1.000000000000000000, 0.000000000000000000, 0.000000000000000000 ) ) ;
#17427 = FACE_OUTER_BOUND ( 'NONE', #5907, .T. ) ;
#17428 = FACE_OUTER_BOUND ( 'NONE', #12804, .T. ) ;
#17429 = LINE ( 'NONE', #6584, #7135 ) ;
#17430 = DIRECTION ( 'NONE',  ( -1.000000000000000000, -0.000000000000000000, -0.000000000000000000 ) ) ;
#17431 = ORIENTED_EDGE ( 'NONE', *, *, #2639, .F. ) ;
#17432 = CARTESIAN_POINT ( 'NONE',  ( 8.680847955711007202, 5.912916378492122225E-13, -4.633165578109188942 ) ) ;
#17433 = ORIENTED_EDGE ( 'NONE', *, *, #8674, .T. ) ;
#17434 = CARTESIAN_POINT ( 'NONE',  ( 23.00000000000000000, -9.374578970469700678, 10.68280860024311885 ) ) ;
#17435 = CARTESIAN_POINT ( 'NONE',  ( 7.685661446562381371, -5.583959896777971110, 11.00674201446023304 ) ) ;
#17436 = EDGE_CURVE ( 'NONE', #5783, #1010, #7132, .T. ) ;
#17437 = ORIENTED_EDGE ( 'NONE', *, *, #10942, .T. ) ;
#17438 = DIRECTION ( 'NONE',  ( 1.000000000000000000, 2.251221844363938350E-33, -6.162975822039154730E-33 ) ) ;
#17439 = CARTESIAN_POINT ( 'NONE',  ( 8.680847955711199049, -2.820578480813074496, -12.53316557810918752 ) ) ;
#17440 = CARTESIAN_POINT ( 'NONE',  ( 28.27483331787888332, -41.23752903419610050, 0.000000000000000000 ) ) ;
#17441 = EDGE_CURVE ( 'NONE', #5565, #1549, #5603, .T. ) ;
#17442 = CARTESIAN_POINT ( 'NONE',  ( -7.685661446562381371, 5.583959896777970222, 6.859589141758143604 ) ) ;
#17443 = DIRECTION ( 'NONE',  ( -0.000000000000000000, 0.000000000000000000, 1.000000000000000000 ) ) ;
#17444 = DIRECTION ( 'NONE',  ( 1.000000000000000000, 0.000000000000000000, 0.000000000000000000 ) ) ;
#17445 = EDGE_CURVE ( 'NONE', #11051, #2256, #6388, .T. ) ;
#17446 = LINE ( 'NONE', #20745, #3580 ) ;
#17447 = FACE_OUTER_BOUND ( 'NONE', #13155, .T. ) ;
#17448 = ORIENTED_EDGE ( 'NONE', *, *, #14379, .T. ) ;
#17449 = EDGE_LOOP ( 'NONE', ( #5169, #927, #995, #15916 ) ) ;
#17450 = FACE_OUTER_BOUND ( 'NONE', #23625, .T. ) ;
#17451 = DIRECTION ( 'NONE',  ( -0.7052211081716897034, -0.7089874389501510388, 0.000000000000000000 ) ) ;
#17452 = CIRCLE ( 'NONE', #10032, 5.099999999999996980 ) ;
#17453 = CARTESIAN_POINT ( 'NONE',  ( -29.00000000000000000, 29.49999999999999645, 0.000000000000000000 ) ) ;
#17454 = CARTESIAN_POINT ( 'NONE',  ( 62.94340820527399671, -5.000000000000000888, 6.123233995736776143E-16 ) ) ;
#17455 = CYLINDRICAL_SURFACE ( 'NONE', #4701, 1.000000000000000888 ) ;
#17456 = ORIENTED_EDGE ( 'NONE', *, *, #23282, .F. ) ;
#17457 = CARTESIAN_POINT ( 'NONE',  ( 29.00000000000000355, 29.50000000000000000, -27.00000000000000000 ) ) ;
#17458 = FACE_OUTER_BOUND ( 'NONE', #4658, .T. ) ;
#17459 = ORIENTED_EDGE ( 'NONE', *, *, #11333, .F. ) ;
#17460 = CARTESIAN_POINT ( 'NONE',  ( 9.500000000000000000, 6.470877716354879437E-13, -7.206742014460234103 ) ) ;
#17461 = ORIENTED_EDGE ( 'NONE', *, *, #20185, .F. ) ;
#17462 = FACE_OUTER_BOUND ( 'NONE', #12103, .T. ) ;
#17463 = CARTESIAN_POINT ( 'NONE',  ( -5.365059087798940141, -7.384370330707086261, 5.933165578109187877 ) ) ;
#17464 = ADVANCED_FACE ( 'NONE', ( #7599, #17006 ), #9555, .F. ) ;
#17465 = DIRECTION ( 'NONE',  ( 0.000000000000000000, 0.000000000000000000, 1.000000000000000000 ) ) ;
#17466 = FACE_OUTER_BOUND ( 'NONE', #16853, .T. ) ;
#17467 = CARTESIAN_POINT ( 'NONE',  ( 2.570122167802765922, 1.191082103573950341E-15, -9.725923461386811297 ) ) ;
#17468 = CARTESIAN_POINT ( 'NONE',  ( 0.000000000000000000, -2.342598717236905603, 4.057500000000010765 ) ) ;
#17469 = EDGE_CURVE ( 'NONE', #1993, #21516, #10709, .T. ) ;
#17470 = VERTEX_POINT ( 'NONE', #20925 ) ;
#17471 = CONTEXT_DEPENDENT_SHAPE_REPRESENTATION ( #17109, #13352 ) ;
#17472 = VERTEX_POINT ( 'NONE', #24090 ) ;
#17473 = CARTESIAN_POINT ( 'NONE',  ( 23.90000000000000568, 29.50000000000000000, -27.00000000000000000 ) ) ;
#17474 = VERTEX_POINT ( 'NONE', #15272 ) ;
#17475 = CARTESIAN_POINT ( 'NONE',  ( -8.835537148983579669, -3.054185505207691165, -12.18395005276799736 ) ) ;
#17476 = FACE_BOUND ( 'NONE', #8179, .T. ) ;
#17477 = VERTEX_POINT ( 'NONE', #4208 ) ;
#17478 = DIRECTION ( 'NONE',  ( -1.000000000000000000, -2.600433232233976523E-16, -0.000000000000000000 ) ) ;
#17479 = ORIENTED_EDGE ( 'NONE', *, *, #7110, .F. ) ;
#17480 = DIRECTION ( 'NONE',  ( -1.000000000000000000, 0.000000000000000000, 0.000000000000000000 ) ) ;
#17481 = DIRECTION ( 'NONE',  ( 1.000000000000000000, 1.224606353822377258E-16, 0.000000000000000000 ) ) ;
#17482 = DIRECTION ( 'NONE',  ( -0.000000000000000000, -0.000000000000000000, -1.000000000000000000 ) ) ;
#17483 = AXIS2_PLACEMENT_3D ( 'NONE', #12435, #15744, #8539 ) ;
#17484 = FACE_OUTER_BOUND ( 'NONE', #11267, .T. ) ;
#17485 = ORIENTED_EDGE ( 'NONE', *, *, #18500, .T. ) ;
#17486 = CARTESIAN_POINT ( 'NONE',  ( 0.000000000000000000, -13.61176534793449200, 4.089617900950054619 ) ) ;
#17487 = DIRECTION ( 'NONE',  ( 0.000000000000000000, 0.000000000000000000, 1.000000000000000000 ) ) ;
#17488 = VERTEX_POINT ( 'NONE', #18718 ) ;
#17489 = ORIENTED_EDGE ( 'NONE', *, *, #5311, .F. ) ;
#17490 = CARTESIAN_POINT ( 'NONE',  ( 9.499999999999790390, 3.086737114213260025, 4.159589141758141650 ) ) ;
#17491 = ORIENTED_EDGE ( 'NONE', *, *, #22099, .T. ) ;
#17492 = ORIENTED_EDGE ( 'NONE', *, *, #6182, .F. ) ;
#17493 = ADVANCED_FACE ( 'NONE', ( #13103 ), #12976, .F. ) ;
#17494 = AXIS2_PLACEMENT_3D ( 'NONE', #12897, #18534, #11282 ) ;
#17495 = EDGE_CURVE ( 'NONE', #23345, #7541, #22749, .T. ) ;
#17496 = ORIENTED_EDGE ( 'NONE', *, *, #216, .F. ) ;
#17497 = EDGE_LOOP ( 'NONE', ( #8707, #18286, #482, #1424, #20402, #23426 ) ) ;
#17498 = CARTESIAN_POINT ( 'NONE',  ( 83.30704456891035647, 7.562528597612068045E-15, 0.000000000000000000 ) ) ;
#17499 = DIRECTION ( 'NONE',  ( -1.000000000000000000, 0.000000000000000000, 0.000000000000000000 ) ) ;
#17500 = CARTESIAN_POINT ( 'NONE',  ( -5.871322893124554021, 8.081182679343978492, 7.906742014460233392 ) ) ;
#17501 = ORIENTED_EDGE ( 'NONE', *, *, #21653, .F. ) ;
#17502 = FACE_OUTER_BOUND ( 'NONE', #947, .T. ) ;
#17503 = DIRECTION ( 'NONE',  ( -1.000000000000000000, 0.000000000000000000, 0.000000000000000000 ) ) ;
#17504 = DIRECTION ( 'NONE',  ( -1.000000000000000000, -1.224606353822377258E-16, -0.000000000000000000 ) ) ;
#17505 = VECTOR ( 'NONE', #15544, 1000.000000000000000 ) ;
#17506 = DIRECTION ( 'NONE',  ( -0.000000000000000000, -0.000000000000000000, -1.000000000000000000 ) ) ;
#17507 = ORIENTED_EDGE ( 'NONE', *, *, #15981, .F. ) ;
#17508 = CARTESIAN_POINT ( 'NONE',  ( 0.000000000000000000, -3.205857990849673378, -11.23818298448545860 ) ) ;
#17509 = EDGE_LOOP ( 'NONE', ( #13794, #1643, #6446, #1570, #9693, #303 ) ) ;
#17510 = CARTESIAN_POINT ( 'NONE',  ( 2.935661446562616295, -9.035036904803758873, 3.659589141758142983 ) ) ;
#17511 = CARTESIAN_POINT ( 'NONE',  ( -36.00000000000000711, -51.00000000000000711, 0.000000000000000000 ) ) ;
#17512 = EDGE_CURVE ( 'NONE', #7020, #6200, #20431, .T. ) ;
#17513 = DIRECTION ( 'NONE',  ( 1.000000000000000000, 0.000000000000000000, 0.000000000000000000 ) ) ;
#17514 = CARTESIAN_POINT ( 'NONE',  ( -6.233975306307045953E-13, 9.127583699786111282, -7.133165578109187166 ) ) ;
#17515 = ORIENTED_EDGE ( 'NONE', *, *, #4635, .F. ) ;
#17516 = EDGE_CURVE ( 'NONE', #9276, #3367, #11875, .T. ) ;
#17517 = FACE_OUTER_BOUND ( 'NONE', #20351, .T. ) ;
#17518 = VERTEX_POINT ( 'NONE', #1994 ) ;
#17519 = ORIENTED_EDGE ( 'NONE', *, *, #1859, .F. ) ;
#17520 = CARTESIAN_POINT ( 'NONE',  ( 6.222797240145152671E-13, -9.127583699786111282, 12.13316557810918717 ) ) ;
#17521 = EDGE_CURVE ( 'NONE', #18614, #3340, #13787, .T. ) ;
#17522 = EDGE_CURVE ( 'NONE', #6942, #17856, #3722, .T. ) ;
#17523 = ADVANCED_FACE ( 'NONE', ( #11361 ), #15152, .T. ) ;
#17524 = VERTEX_POINT ( 'NONE', #11135 ) ;
#17525 = DIRECTION ( 'NONE',  ( 0.000000000000000000, 0.000000000000000000, 1.000000000000000000 ) ) ;
#17526 = DIRECTION ( 'NONE',  ( 1.000000000000000000, -0.000000000000000000, -0.000000000000000000 ) ) ;
#17527 = VERTEX_POINT ( 'NONE', #19086 ) ;
#17528 = CARTESIAN_POINT ( 'NONE',  ( 33.99999999999998579, -6.000000000000013323, 12.00000000000000000 ) ) ;
#17529 = FACE_OUTER_BOUND ( 'NONE', #10239, .T. ) ;
#17530 = CIRCLE ( 'NONE', #3120, 5.000000000000007994 ) ;
#17531 = CARTESIAN_POINT ( 'NONE',  ( -2.935661446561384391, -9.035036904804158553, -10.60674201446023446 ) ) ;
#17532 = DIRECTION ( 'NONE',  ( -1.000000000000000000, -0.000000000000000000, -0.000000000000000000 ) ) ;
#17533 = FACE_OUTER_BOUND ( 'NONE', #11346, .T. ) ;
#17534 = VERTEX_POINT ( 'NONE', #13337 ) ;
#17535 = DIRECTION ( 'NONE',  ( 0.000000000000000000, 0.000000000000000000, 1.000000000000000000 ) ) ;
#17536 = CARTESIAN_POINT ( 'NONE',  ( -9.500000000000000000, 0.000000000000000000, 12.50000000000000000 ) ) ;
#17537 = DIRECTION ( 'NONE',  ( 1.000000000000000000, 0.000000000000000000, 0.000000000000000000 ) ) ;
#17538 = FACE_OUTER_BOUND ( 'NONE', #3607, .T. ) ;
#17539 = DIRECTION ( 'NONE',  ( -0.000000000000000000, -0.000000000000000000, -1.000000000000000000 ) ) ;
#17540 = FACE_OUTER_BOUND ( 'NONE', #20296, .T. ) ;
#17541 = EDGE_CURVE ( 'NONE', #5671, #12632, #18609, .T. ) ;
#17542 = DIRECTION ( 'NONE',  ( -5.501724186093585079E-16, -1.000000000000000000, 0.000000000000000000 ) ) ;
#17543 = ORIENTED_EDGE ( 'NONE', *, *, #6657, .T. ) ;
#17544 = CARTESIAN_POINT ( 'NONE',  ( -7.022953521754877748, -5.102474405760673015, -3.833165578109188676 ) ) ;
#17545 = EDGE_CURVE ( 'NONE', #17470, #12988, #22265, .T. ) ;
#17546 = ORIENTED_EDGE ( 'NONE', *, *, #3764, .F. ) ;
#17547 = VECTOR ( 'NONE', #7689, 1000.000000000000000 ) ;
#17548 = DIRECTION ( 'NONE',  ( -1.000000000000000000, -0.000000000000000000, -0.000000000000000000 ) ) ;
#17549 = SPHERICAL_SURFACE ( 'NONE', #4680, 1.000000000000000000 ) ;
#17550 = ADVANCED_FACE ( 'NONE', ( #6031 ), #20797, .F. ) ;
#17551 = ORIENTED_EDGE ( 'NONE', *, *, #4550, .T. ) ;
#17552 = CYLINDRICAL_SURFACE ( 'NONE', #23942, 6.050000000006051870 ) ;
#17553 = CARTESIAN_POINT ( 'NONE',  ( 0.3000000000000020983, 0.000000000000000000, 0.000000000000000000 ) ) ;
#17554 = CARTESIAN_POINT ( 'NONE',  ( 0.000000000000000000, -15.03999999999999915, -25.00000000000000000 ) ) ;
#17555 = CARTESIAN_POINT ( 'NONE',  ( 7.937578510445243651, -3.514536757623948127, -12.49999999999998046 ) ) ;
#17556 = DIRECTION ( 'NONE',  ( 0.000000000000000000, -1.000000000000000000, 0.000000000000000000 ) ) ;
#17557 = CARTESIAN_POINT ( 'NONE',  ( 5.871322893123449127, 8.081182679344781405, -4.359589141758143604 ) ) ;
#17558 = ORIENTED_EDGE ( 'NONE', *, *, #7798, .F. ) ;
#17559 = CYLINDRICAL_SURFACE ( 'NONE', #11743, 8.999999999999994671 ) ;
#17560 = ORIENTED_EDGE ( 'NONE', *, *, #10304, .T. ) ;
#17561 = DIRECTION ( 'NONE',  ( -1.000000000000000000, -1.224606353822377258E-16, -0.000000000000000000 ) ) ;
#17562 = DIRECTION ( 'NONE',  ( 0.7089874389501514829, -0.7052211081716890373, 0.000000000000000000 ) ) ;
#17563 = LINE ( 'NONE', #12063, #12179 ) ;
#17564 = CARTESIAN_POINT ( 'NONE',  ( 41.73082370883260239, 27.62204025492844650, 0.000000000000000000 ) ) ;
#17565 = FACE_OUTER_BOUND ( 'NONE', #5448, .T. ) ;
#17566 = ADVANCED_FACE ( 'NONE', ( #420 ), #11619, .F. ) ;
#17567 = VERTEX_POINT ( 'NONE', #65 ) ;
#17568 = CARTESIAN_POINT ( 'NONE',  ( 5.378177448618336243, 0.000000000000000000, 10.94716442891539465 ) ) ;
#17569 = CARTESIAN_POINT ( 'NONE',  ( 69.63636363636364024, 7.491529369508391930E-15, 0.000000000000000000 ) ) ;
#17570 = ORIENTED_EDGE ( 'NONE', *, *, #2362, .T. ) ;
#17571 = CARTESIAN_POINT ( 'NONE',  ( -2.935661446561384391, -9.035036904804158553, -8.606742014460234458 ) ) ;
#17572 = ORIENTED_EDGE ( 'NONE', *, *, #24074, .F. ) ;
#17573 = CARTESIAN_POINT ( 'NONE',  ( 30.32370777929697780, -42.16181938034194587, 0.000000000000000000 ) ) ;
#17574 = CARTESIAN_POINT ( 'NONE',  ( 2.682529543899157876, 8.255977015246598327, 9.033165578109187521 ) ) ;
#17575 = EDGE_CURVE ( 'NONE', #14151, #13806, #21246, .T. ) ;
#17576 = CYLINDRICAL_SURFACE ( 'NONE', #14686, 8.000000000000000000 ) ;
#17577 = DIRECTION ( 'NONE',  ( -1.000000000000000000, 0.000000000000000000, 0.000000000000000000 ) ) ;
#17578 = AXIS2_PLACEMENT_3D ( 'NONE', #11821, #2583, #9994 ) ;
#17579 =( REPRESENTATION_RELATIONSHIP ('NONE','NONE', #21748, #1013 ) REPRESENTATION_RELATIONSHIP_WITH_TRANSFORMATION ( #4805 )SHAPE_REPRESENTATION_RELATIONSHIP( ) );
#17580 = CIRCLE ( 'NONE', #13284, 4.499999999999997335 ) ;
#17581 = VECTOR ( 'NONE', #22294, 1000.000000000000000 ) ;
#17582 = ORIENTED_EDGE ( 'NONE', *, *, #15829, .T. ) ;
#17583 = VERTEX_POINT ( 'NONE', #2490 ) ;
#17584 = DIRECTION ( 'NONE',  ( -0.000000000000000000, -0.000000000000000000, -1.000000000000000000 ) ) ;
#17585 = CARTESIAN_POINT ( 'NONE',  ( -5.871322893124554021, 8.081182679343978492, -11.90674201446023339 ) ) ;
#17586 = ORIENTED_EDGE ( 'NONE', *, *, #21530, .F. ) ;
#17587 = ORIENTED_EDGE ( 'NONE', *, *, #5495, .T. ) ;
#17588 = CARTESIAN_POINT ( 'NONE',  ( 83.30704456891035647, 7.562528597612068045E-15, 0.000000000000000000 ) ) ;
#17589 = ADVANCED_FACE ( 'NONE', ( #4323 ), #6150, .F. ) ;
#17590 = CARTESIAN_POINT ( 'NONE',  ( 60.03431729618309021, 5.000000000000015987, 0.000000000000000000 ) ) ;
#17591 = ORIENTED_EDGE ( 'NONE', *, *, #1717, .T. ) ;
#17592 = CARTESIAN_POINT ( 'NONE',  ( 29.00000000000000000, 29.50000000000000000, 14.00000000000000178 ) ) ;
#17593 = AXIS2_PLACEMENT_3D ( 'NONE', #605, #5841, #6089 ) ;
#17594 = EDGE_CURVE ( 'NONE', #9993, #15508, #20033, .T. ) ;
#17595 = ORIENTED_EDGE ( 'NONE', *, *, #14039, .F. ) ;
#17596 = FACE_OUTER_BOUND ( 'NONE', #22996, .T. ) ;
#17597 = PLANE ( 'NONE',  #18414 ) ;
#17598 = VECTOR ( 'NONE', #15039, 1000.000000000000000 ) ;
#17599 = DIRECTION ( 'NONE',  ( 0.000000000000000000, 0.000000000000000000, 1.000000000000000000 ) ) ;
#17600 = CARTESIAN_POINT ( 'NONE',  ( 71.67068093254673045, 7.562528597612068045E-15, 0.000000000000000000 ) ) ;
#17601 = ORIENTED_EDGE ( 'NONE', *, *, #8470, .T. ) ;
#17602 = DIRECTION ( 'NONE',  ( 0.000000000000000000, 0.000000000000000000, 1.000000000000000000 ) ) ;
#17603 = DIRECTION ( 'NONE',  ( -1.000000000000000000, 0.000000000000000000, 0.000000000000000000 ) ) ;
#17604 = FACE_OUTER_BOUND ( 'NONE', #1094, .T. ) ;
#17605 = ORIENTED_EDGE ( 'NONE', *, *, #815, .F. ) ;
#17606 = CARTESIAN_POINT ( 'NONE',  ( 9.499999999999790390, 3.086737114213260025, 6.159589141758145203 ) ) ;
#17607 = VERTEX_POINT ( 'NONE', #2620 ) ;
#17608 = ORIENTED_EDGE ( 'NONE', *, *, #23483, .T. ) ;
#17609 = VECTOR ( 'NONE', #10807, 1000.000000000000000 ) ;
#17610 = ORIENTED_EDGE ( 'NONE', *, *, #2156, .F. ) ;
#17611 = VECTOR ( 'NONE', #8951, 1000.000000000000000 ) ;
#17612 = AXIS2_PLACEMENT_3D ( 'NONE', #15385, #6132, #17577 ) ;
#17613 = DIRECTION ( 'NONE',  ( -1.000000000000000000, -1.224606353822377258E-16, -0.000000000000000000 ) ) ;
#17615 = AXIS2_PLACEMENT_3D ( 'NONE', #7530, #10944, #20368 ) ;
#17614 = CARTESIAN_POINT ( 'NONE',  ( 6.222797240145152671E-13, -9.127583699786111282, -6.133165578109188942 ) ) ;
#17616 = AXIS2_PLACEMENT_3D ( 'NONE', #2439, #17322, #22951 ) ;
#17617 = CIRCLE ( 'NONE', #20743, 5.100000000000000533 ) ;
#17618 = FACE_OUTER_BOUND ( 'NONE', #2730, .T. ) ;
#17619 = CARTESIAN_POINT ( 'NONE',  ( -7.685661446562381371, 5.583959896777970222, -6.006742014460233037 ) ) ;
#17620 = ORIENTED_EDGE ( 'NONE', *, *, #19932, .F. ) ;
#17621 = CARTESIAN_POINT ( 'NONE',  ( -16.08510323282434129, -6.088885580147182175, 7.295537496892092300 ) ) ;
#17622 = CARTESIAN_POINT ( 'NONE',  ( 74.00000000000001421, 7.491529369508391930E-15, 0.000000000000000000 ) ) ;
#17623 = VECTOR ( 'NONE', #23722, 1000.000000000000000 ) ;
#17624 = DIRECTION ( 'NONE',  ( 1.000000000000000000, 0.000000000000000000, 0.000000000000000000 ) ) ;
#17625 = VERTEX_POINT ( 'NONE', #11869 ) ;
#17626 = DIRECTION ( 'NONE',  ( -1.000000000000000000, -0.000000000000000000, -0.000000000000000000 ) ) ;
#17627 = DIRECTION ( 'NONE',  ( 0.000000000000000000, 0.000000000000000000, 1.000000000000000000 ) ) ;
#17628 = EDGE_CURVE ( 'NONE', #9926, #14186, #21208, .T. ) ;
#17629 = EDGE_CURVE ( 'NONE', #15211, #21933, #6790, .T. ) ;
#17630 = FACE_OUTER_BOUND ( 'NONE', #17449, .T. ) ;
#17631 = CARTESIAN_POINT ( 'NONE',  ( -2.935661446562617183, 9.035036904803758873, 4.659589141758143427 ) ) ;
#17632 = CARTESIAN_POINT ( 'NONE',  ( 17.15849686392982676, -8.309918483244977949, 4.628645577532783051 ) ) ;
#17633 = CIRCLE ( 'NONE', #8659, 9.000000000000000000 ) ;
#17634 = CARTESIAN_POINT ( 'NONE',  ( 14.51962751333974389, 3.765689428759029234, 8.721787840009197268 ) ) ;
#17635 = CARTESIAN_POINT ( 'NONE',  ( -8.680847955711200825, 2.820578480813073607, -7.533165578109189298 ) ) ;
#17636 = AXIS2_PLACEMENT_3D ( 'NONE', #263, #22687, #1947 ) ;
#17637 = AXIS2_PLACEMENT_3D ( 'NONE', #9996, #2947, #15604 ) ;
#17638 = ORIENTED_EDGE ( 'NONE', *, *, #12455, .T. ) ;
#17639 = AXIS2_PLACEMENT_3D ( 'NONE', #2091, #9517, #7564 ) ;
#17640 = DIRECTION ( 'NONE',  ( -1.000000000000000000, -1.224606353822377258E-16, -0.000000000000000000 ) ) ;
#17641 = ORIENTED_EDGE ( 'NONE', *, *, #12223, .F. ) ;
#17642 = VERTEX_POINT ( 'NONE', #17372 ) ;
#17643 = AXIS2_PLACEMENT_3D ( 'NONE', #22116, #16462, #12808 ) ;
#17644 = CARTESIAN_POINT ( 'NONE',  ( 2.682529543900284974, -8.255977015246234174, 12.23316557810919036 ) ) ;
#17645 = VECTOR ( 'NONE', #321, 1000.000000000000000 ) ;
#17646 = ORIENTED_EDGE ( 'NONE', *, *, #13348, .T. ) ;
#17647 = DIRECTION ( 'NONE',  ( 0.3085117869262298251, 0.9512205198205011536, 1.956743869958810036E-15 ) ) ;
#17648 = CARTESIAN_POINT ( 'NONE',  ( 0.000000000000000000, 0.000000000000000000, 0.000000000000000000 ) ) ;
#17649 = VERTEX_POINT ( 'NONE', #15909 ) ;
#17650 = DIRECTION ( 'NONE',  ( -0.000000000000000000, -0.000000000000000000, -1.000000000000000000 ) ) ;
#17651 = UNCERTAINTY_MEASURE_WITH_UNIT (LENGTH_MEASURE( 1.000000000000000082E-05 ), #22675, 'distance_accuracy_value', 'NONE');
#17652 = EDGE_CURVE ( 'NONE', #17850, #17766, #14948, .T. ) ;
#17653 = CARTESIAN_POINT ( 'NONE',  ( 3.000000000000003997, 8.485281374238569541, 99.19971821973399528 ) ) ;
#17654 = CARTESIAN_POINT ( 'NONE',  ( 14.51962751333974389, 3.765689428759029234, -27.00000000000000000 ) ) ;
#17655 = DIRECTION ( 'NONE',  ( 1.000000000000000000, 1.224606353822377258E-16, 0.000000000000000000 ) ) ;
#17656 = AXIS2_PLACEMENT_3D ( 'NONE', #20465, #13131, #3866 ) ;
#17657 = CIRCLE ( 'NONE', #23907, 2.024999999999999911 ) ;
#17658 = ORIENTED_EDGE ( 'NONE', *, *, #11736, .F. ) ;
#17659 = CONICAL_SURFACE ( 'NONE', #14161, 4.171999999999999709, 0.7853981633974687071 ) ;
#17660 = EDGE_CURVE ( 'NONE', #3712, #7231, #8726, .T. ) ;
#17661 = CARTESIAN_POINT ( 'NONE',  ( 33.99999999999998579, 4.999999999999985789, 9.500000000000000000 ) ) ;
#17662 = VERTEX_POINT ( 'NONE', #1043 ) ;
#17663 = CIRCLE ( 'NONE', #6771, 1.024999999999999911 ) ;
#17664 = EDGE_CURVE ( 'NONE', #14048, #19008, #8196, .T. ) ;
#17665 = CARTESIAN_POINT ( 'NONE',  ( -37.00000000000000711, 29.49999999999999645, 11.50000000000000000 ) ) ;
#17666 = EDGE_CURVE ( 'NONE', #23706, #16325, #10146, .T. ) ;
#17667 = EDGE_LOOP ( 'NONE', ( #4457, #1502, #8269, #17174 ) ) ;
#17668 = FACE_OUTER_BOUND ( 'NONE', #17280, .T. ) ;
#17669 = DIRECTION ( 'NONE',  ( -0.000000000000000000, -0.000000000000000000, -1.000000000000000000 ) ) ;
#17670 = CIRCLE ( 'NONE', #12586, 4.000000000000000000 ) ;
#17671 = DIRECTION ( 'NONE',  ( 1.000000000000000000, -0.000000000000000000, -0.000000000000000000 ) ) ;
#17672 = LINE ( 'NONE', #973, #18855 ) ;
#17673 = ORIENTED_EDGE ( 'NONE', *, *, #9392, .F. ) ;
#17674 = CARTESIAN_POINT ( 'NONE',  ( -5.365059087798939252, -7.384370330707086261, -3.933165578109188321 ) ) ;
#17675 = ORIENTED_EDGE ( 'NONE', *, *, #20721, .T. ) ;
#17676 = ORIENTED_EDGE ( 'NONE', *, *, #4742, .F. ) ;
#17677 = CIRCLE ( 'NONE', #23528, 0.9999999999999994449 ) ;
#17678 = CARTESIAN_POINT ( 'NONE',  ( 2.935661446562616295, -9.035036904803758873, 3.659589141758142983 ) ) ;
#17679 = CARTESIAN_POINT ( 'NONE',  ( 5.871322893124553133, -8.081182679343980269, 10.90674201446023339 ) ) ;
#17680 = B_SPLINE_CURVE_WITH_KNOTS ( 'NONE', 3,
 ( #9070, #13293, #15118, #4043, #11458, #18934, #2213, #9636, #7791, #16964, #20999, #4178, #13558, #7681, #16391, #5992 ),
 .UNSPECIFIED., .F., .F.,
 ( 4, 2, 2, 2, 2, 2, 2, 4 ),
 ( 0.000000000000000000, 0.0005906230073307718129, 0.001181246014661543626, 0.001771869021992315439, 0.002362492029323087252, 0.003543738043984660368, 0.004134361051315447143, 0.004724984058646233484 ),
 .UNSPECIFIED. ) ;
#17681 = ORIENTED_EDGE ( 'NONE', *, *, #2798, .T. ) ;
#17682 = DIRECTION ( 'NONE',  ( -6.162975822039154730E-33, -1.232595164407830946E-32, 0.9999999999999997780 ) ) ;
#17683 = VECTOR ( 'NONE', #20673, 1000.000000000000000 ) ;
#17684 = CARTESIAN_POINT ( 'NONE',  ( 33.25000000000000000, 29.50000000000000000, -3.000000000000000000 ) ) ;
#17685 = AXIS2_PLACEMENT_3D ( 'NONE', #7429, #23623, #14318 ) ;
#17686 = DIRECTION ( 'NONE',  ( -1.000000000000000000, 0.000000000000000000, 0.000000000000000000 ) ) ;
#17687 = CIRCLE ( 'NONE', #9102, 1.000000000000000888 ) ;
#17688 = LINE ( 'NONE', #18052, #22460 ) ;
#17689 = DIRECTION ( 'NONE',  ( 0.000000000000000000, -1.000000000000000000, 0.000000000000000000 ) ) ;
#17690 = EDGE_CURVE ( 'NONE', #21150, #17838, #21525, .T. ) ;
#17691 = DIRECTION ( 'NONE',  ( -1.000000000000000000, -1.224606353822377258E-16, -0.000000000000000000 ) ) ;
#17692 = ORIENTED_EDGE ( 'NONE', *, *, #17849, .F. ) ;
#17693 = DIRECTION ( 'NONE',  ( 0.000000000000000000, 1.000000000000000000, -0.000000000000000000 ) ) ;
#17694 = ADVANCED_FACE ( 'NONE', ( #6262 ), #14075, .F. ) ;
#17695 = EDGE_CURVE ( 'NONE', #18698, #19098, #2500, .T. ) ;
#17696 = VERTEX_POINT ( 'NONE', #12098 ) ;
#17697 = DIRECTION ( 'NONE',  ( -1.000000000000000000, -1.224606353822377258E-16, -0.000000000000000000 ) ) ;
#17698 = CARTESIAN_POINT ( 'NONE',  ( -9.378401895172215674, 3.550564238312661509E-15, 12.12159810482778077 ) ) ;
#17699 = DIRECTION ( 'NONE',  ( -1.000000000000000000, 0.000000000000000000, 0.000000000000000000 ) ) ;
#17700 = CARTESIAN_POINT ( 'NONE',  ( 9.366788983124298085, -0.5939584231415685478, 12.13321101687573922 ) ) ;
#17701 = AXIS2_PLACEMENT_3D ( 'NONE', #18519, #7165, #14361 ) ;
#17702 = VECTOR ( 'NONE', #11809, 1000.000000000000114 ) ;
#17703 = CARTESIAN_POINT ( 'NONE',  ( -36.00000000000001421, 50.99999999999999289, 0.000000000000000000 ) ) ;
#17704 = ORIENTED_EDGE ( 'NONE', *, *, #7730, .F. ) ;
#17705 = CONICAL_SURFACE ( 'NONE', #7182, 5.000000000000007994, 0.9599310885968855844 ) ;
#17706 = CONICAL_SURFACE ( 'NONE', #8344, 5.000000000000007994, 0.9599310885968855844 ) ;
#17707 = CARTESIAN_POINT ( 'NONE',  ( 0.000000000000000000, 14.21257171757157245, 6.139082186136624486 ) ) ;
#17708 = ORIENTED_EDGE ( 'NONE', *, *, #18380, .F. ) ;
#17709 = CYLINDRICAL_SURFACE ( 'NONE', #2904, 4.999999999999997335 ) ;
#17710 = AXIS2_PLACEMENT_3D ( 'NONE', #12408, #21703, #21343 ) ;
#17711 = ORIENTED_EDGE ( 'NONE', *, *, #4884, .F. ) ;
#17712 = DIRECTION ( 'NONE',  ( -0.000000000000000000, -0.000000000000000000, -1.000000000000000000 ) ) ;
#17713 = CARTESIAN_POINT ( 'NONE',  ( -5.365059087799948223, 7.384370330706355290, 5.333165578109190008 ) ) ;
#17714 = DIRECTION ( 'NONE',  ( -0.4828336235133043330, -0.8757121056631641531, 0.000000000000000000 ) ) ;
#17715 = DIRECTION ( 'NONE',  ( -1.000000000000000000, -1.224606353822377258E-16, -0.000000000000000000 ) ) ;
#17716 = CARTESIAN_POINT ( 'NONE',  ( 5.378177448618336243, 0.000000000000000000, 0.000000000000000000 ) ) ;
#17717 = CARTESIAN_POINT ( 'NONE',  ( 84.76159002345582394, 5.000000000000015099, 0.000000000000000000 ) ) ;
#17718 = AXIS2_PLACEMENT_3D ( 'NONE', #3979, #7855, #18636 ) ;
#17719 = AXIS2_PLACEMENT_3D ( 'NONE', #1495, #23699, #7072 ) ;
#17720 = VERTEX_POINT ( 'NONE', #15784 ) ;
#17721 = ORIENTED_EDGE ( 'NONE', *, *, #4061, .T. ) ;
#17722 = DIRECTION ( 'NONE',  ( -1.000000000000000000, 0.000000000000000000, 0.000000000000000000 ) ) ;
#17723 = AXIS2_PLACEMENT_3D ( 'NONE', #225, #3982, #11163 ) ;
#17724 = CARTESIAN_POINT ( 'NONE',  ( -7.685661446561619314, -5.583959896779019161, -11.25958914175814307 ) ) ;
#17725 = ORIENTED_EDGE ( 'NONE', *, *, #7246, .F. ) ;
#17726 = CIRCLE ( 'NONE', #23596, 1.999999999999996669 ) ;
#17727 = VERTEX_POINT ( 'NONE', #4586 ) ;
#17728 = EDGE_CURVE ( 'NONE', #16483, #23756, #4067, .T. ) ;
#17729 = DIRECTION ( 'NONE',  ( 1.000000000000000000, 0.000000000000000000, 0.000000000000000000 ) ) ;
#17730 = ORIENTED_EDGE ( 'NONE', *, *, #7719, .T. ) ;
#17731 = LINE ( 'NONE', #1148, #13169 ) ;
#17732 = AXIS2_PLACEMENT_3D ( 'NONE', #23523, #15946, #6805 ) ;
#17733 = AXIS2_PLACEMENT_3D ( 'NONE', #22666, #21338, #12027 ) ;
#17734 = ORIENTED_EDGE ( 'NONE', *, *, #12571, .F. ) ;
#17735 = CARTESIAN_POINT ( 'NONE',  ( -23.85000000000000142, 15.03999999999999737, 2.200000000000000178 ) ) ;
#17736 = DIRECTION ( 'NONE',  ( 0.9160001545545232160, -0.4011779117250717785, 0.000000000000000000 ) ) ;
#17737 = CARTESIAN_POINT ( 'NONE',  ( 82.72727272727273373, 4.172000000000015696, 0.000000000000000000 ) ) ;
#17738 = CARTESIAN_POINT ( 'NONE',  ( 0.000000000000000000, 0.000000000000000000, 11.99999999999999645 ) ) ;
#17739 = ORIENTED_EDGE ( 'NONE', *, *, #7425, .F. ) ;
#17740 = APPLICATION_CONTEXT ( 'automotive_design' ) ;
#17741 = FACE_OUTER_BOUND ( 'NONE', #6993, .T. ) ;
#17742 = FACE_OUTER_BOUND ( 'NONE', #7773, .T. ) ;
#17743 = DIRECTION ( 'NONE',  ( -1.000000000000000000, -1.224606353822377258E-16, -0.000000000000000000 ) ) ;
#17744 = ORIENTED_EDGE ( 'NONE', *, *, #18947, .T. ) ;
#17745 = CIRCLE ( 'NONE', #12282, 5.000000000000007994 ) ;
#17746 = CARTESIAN_POINT ( 'NONE',  ( 2.935661446562616295, -9.035036904803758873, 5.659589141758144315 ) ) ;
#17747 = VECTOR ( 'NONE', #4767, 1000.000000000000000 ) ;
#17748 = ORIENTED_EDGE ( 'NONE', *, *, #8058, .T. ) ;
#17749 = ADVANCED_FACE ( 'NONE', ( #17741 ), #19709, .F. ) ;
#17750 = TOROIDAL_SURFACE ( 'NONE', #4565, 3.500000000000001776, 1.500000000000000000 ) ;
#17751 = VECTOR ( 'NONE', #3539, 1000.000000000000000 ) ;
#17752 = PRESENTATION_LAYER_ASSIGNMENT (  '', '', ( #1007 ) ) ;
#17753 = B_SPLINE_CURVE_WITH_KNOTS ( 'NONE', 3,
 ( #9871, #4290, #8046, #17197, #21110, #15490, #22957, #6354, #2811, #13796, #15229, #21245, #6227, #4413, #13556, #23204, #10241, #11952, #11581, #19056, #2328, #19419, #20998, #11822, #2696, #17698 ),
 .UNSPECIFIED., .F., .F.,
 ( 4, 2, 2, 2, 2, 2, 2, 2, 2, 2, 2, 2, 4 ),
 ( 0.000000000000000000, 0.001163219550936220315, 0.002326439101872440629, 0.004652878203744879523, 0.005816097754681098971, 0.006979317305617317550, 0.008142536856553536997, 0.009305756407489757312, 0.01163219550936219794, 0.01395863461123463684, 0.01512185416217085715, 0.01628507371310707399, 0.01861151281497951115 ),
 .UNSPECIFIED. ) ;
#17754 = ORIENTED_EDGE ( 'NONE', *, *, #17664, .T. ) ;
#17755 = ORIENTED_EDGE ( 'NONE', *, *, #6444, .T. ) ;
#17756 = EDGE_CURVE ( 'NONE', #2429, #4017, #23251, .T. ) ;
#17757 = DIRECTION ( 'NONE',  ( -0.5735764363510517105, -0.8191520442889879128, 0.000000000000000000 ) ) ;
#17758 = DIRECTION ( 'NONE',  ( -1.000000000000000000, 0.000000000000000000, 0.000000000000000000 ) ) ;
#17759 = ADVANCED_FACE ( 'NONE', ( #6528 ), #4455, .F. ) ;
#17760 = DIRECTION ( 'NONE',  ( -1.000000000000000000, 0.000000000000000000, 0.000000000000000000 ) ) ;
#17761 = ORIENTED_EDGE ( 'NONE', *, *, #9747, .F. ) ;
#17762 = CARTESIAN_POINT ( 'NONE',  ( -16.81886298599061647, -7.518780870797758809, 5.825851398835388828 ) ) ;
#17763 = ADVANCED_FACE ( 'NONE', ( #9775 ), #543, .F. ) ;
#17764 = AXIS2_PLACEMENT_3D ( 'NONE', #6573, #4872, #4626 ) ;
#17765 = CARTESIAN_POINT ( 'NONE',  ( 3.000000000000002665, 111.0000000000000000, 98.99999999999998579 ) ) ;
#17766 = VERTEX_POINT ( 'NONE', #3212 ) ;
#17767 = DIRECTION ( 'NONE',  ( -0.000000000000000000, -0.000000000000000000, 1.000000000000000000 ) ) ;
#17768 = AXIS2_PLACEMENT_3D ( 'NONE', #4026, #11443, #18918 ) ;
#17769 = DIRECTION ( 'NONE',  ( 1.000000000000000000, 0.000000000000000000, 0.000000000000000000 ) ) ;
#17771 = LINE ( 'NONE', #8719, #10616 ) ;
#17770 = CIRCLE ( 'NONE', #1791, 5.000000000000007994 ) ;
#17772 = CARTESIAN_POINT ( 'NONE',  ( 41.00000000000000000, 5.999999999999986677, 11.00000000000000000 ) ) ;
#17773 = AXIS2_PLACEMENT_3D ( 'NONE', #8717, #3008, #16166 ) ;
#17774 = FACE_OUTER_BOUND ( 'NONE', #2246, .T. ) ;
#17775 = CARTESIAN_POINT ( 'NONE',  ( 7.022953521754877748, 5.102474405760673903, -10.83316557810919001 ) ) ;
#17776 = VECTOR ( 'NONE', #3592, 1000.000000000000000 ) ;
#17777 = CARTESIAN_POINT ( 'NONE',  ( 23.97500000000000497, 29.50000000000000000, -3.000000000000000000 ) ) ;
#17778 = LINE ( 'NONE', #13875, #11422 ) ;
#17779 = CARTESIAN_POINT ( 'NONE',  ( 5.365059087799947335, -7.384370330706356178, -10.33316557810918823 ) ) ;
#17780 = CARTESIAN_POINT ( 'NONE',  ( 69.63636363636364024, 7.491529369508391930E-15, 0.000000000000000000 ) ) ;
#17781 = ORIENTED_EDGE ( 'NONE', *, *, #10015, .F. ) ;
#17782 = ORIENTED_EDGE ( 'NONE', *, *, #3786, .F. ) ;
#17783 = CARTESIAN_POINT ( 'NONE',  ( -5.622572944242076564E-13, 8.680847955711007202, 3.133165578109187166 ) ) ;
#17784 = AXIS2_PLACEMENT_3D ( 'NONE', #7489, #11151, #437 ) ;
#17785 = ORIENTED_EDGE ( 'NONE', *, *, #16794, .T. ) ;
#17786 = DIRECTION ( 'NONE',  ( 1.000000000000000000, 0.000000000000000000, 0.000000000000000000 ) ) ;
#17787 = AXIS2_PLACEMENT_3D ( 'NONE', #2898, #19746, #21799 ) ;
#17788 = CARTESIAN_POINT ( 'NONE',  ( 2.935661446561383503, 9.035036904804158553, -11.60674201446023268 ) ) ;
#17789 = AXIS2_PLACEMENT_3D ( 'NONE', #827, #9954, #4740 ) ;
#17790 = ORIENTED_EDGE ( 'NONE', *, *, #19185, .F. ) ;
#17791 = EDGE_CURVE ( 'NONE', #11663, #22613, #10869, .T. ) ;
#17792 = DIRECTION ( 'NONE',  ( 1.000000000000000000, 0.000000000000000000, 0.000000000000000000 ) ) ;
#17793 = CARTESIAN_POINT ( 'NONE',  ( 70.51113724927145654, 7.420530141404717394E-15, 0.000000000000000000 ) ) ;
#17794 = EDGE_CURVE ( 'NONE', #8782, #21563, #18468, .T. ) ;
#17795 = AXIS2_PLACEMENT_3D ( 'NONE', #13815, #12212, #21629 ) ;
#17796 = CARTESIAN_POINT ( 'NONE',  ( -6.153822176767817416E-13, 9.500000000000000000, 2.873059427838761781 ) ) ;
#17797 = FACE_OUTER_BOUND ( 'NONE', #18752, .T. ) ;
#17798 = CARTESIAN_POINT ( 'NONE',  ( 81.85249911436491743, 7.562528597612068045E-15, 0.000000000000000000 ) ) ;
#17799 = ORIENTED_EDGE ( 'NONE', *, *, #23686, .F. ) ;
#17800 = DIRECTION ( 'NONE',  ( -0.000000000000000000, -0.000000000000000000, -1.000000000000000000 ) ) ;
#17801 = CARTESIAN_POINT ( 'NONE',  ( -1.999999999999994449, 45.00000000000000000, -26.97499999999999432 ) ) ;
#17802 = VERTEX_POINT ( 'NONE', #18109 ) ;
#17803 = AXIS2_PLACEMENT_3D ( 'NONE', #8213, #21050, #22898 ) ;
#17804 = CARTESIAN_POINT ( 'NONE',  ( -34.00000000000000000, -3.851859888774471706E-31, 10.49999999999999822 ) ) ;
#17805 = CARTESIAN_POINT ( 'NONE',  ( 78.94340820527399671, 5.000000000000015987, 0.000000000000000000 ) ) ;
#17806 = DIRECTION ( 'NONE',  ( 1.000000000000000000, 0.000000000000000000, 0.000000000000000000 ) ) ;
#17807 = VECTOR ( 'NONE', #19718, 1000.000000000000114 ) ;
#17808 = CARTESIAN_POINT ( 'NONE',  ( 34.10000000000000142, -29.50000000000000355, 0.000000000000000000 ) ) ;
#17809 = ORIENTED_EDGE ( 'NONE', *, *, #20280, .T. ) ;
#17810 = CARTESIAN_POINT ( 'NONE',  ( -2.682529543900285862, 8.255977015246234174, -5.233165578109188587 ) ) ;
#17811 = VECTOR ( 'NONE', #4897, 1000.000000000000000 ) ;
#17812 = VERTEX_POINT ( 'NONE', #1404 ) ;
#17813 = EDGE_CURVE ( 'NONE', #4495, #16085, #17983, .T. ) ;
#17814 = ORIENTED_EDGE ( 'NONE', *, *, #4500, .T. ) ;
#17815 = CARTESIAN_POINT ( 'NONE',  ( -9.500000000000000000, -6.482511860946779655E-13, 5.059589141758143782 ) ) ;
#17816 = CARTESIAN_POINT ( 'NONE',  ( -9.499999999999790390, -3.086737114213257804, 10.30674201446023375 ) ) ;
#17817 = ORIENTED_EDGE ( 'NONE', *, *, #6603, .T. ) ;
#17818 =( LENGTH_UNIT ( ) NAMED_UNIT ( * ) SI_UNIT ( .MILLI., .METRE. ) );
#17819 = EDGE_CURVE ( 'NONE', #7640, #8629, #1158, .T. ) ;
#17820 = CARTESIAN_POINT ( 'NONE',  ( 0.000000000000000000, -45.00000000000000000, -27.00000000000000000 ) ) ;
#17821 = ADVANCED_FACE ( 'NONE', ( #12829 ), #8340, .T. ) ;
#17822 = CARTESIAN_POINT ( 'NONE',  ( 58.57977184163763695, -5.000000000000000000, 6.123233995736775157E-16 ) ) ;
#17823 = CARTESIAN_POINT ( 'NONE',  ( 9.500000000000000000, 6.470877716354879437E-13, 6.059589141758143782 ) ) ;
#17824 = EDGE_CURVE ( 'NONE', #14019, #11511, #244, .T. ) ;
#17825 = CIRCLE ( 'NONE', #15864, 4.172000000000008590 ) ;
#17826 = CIRCLE ( 'NONE', #10348, 6.050000000006050982 ) ;
#17827 = FILL_AREA_STYLE_COLOUR ( '', #24023 ) ;
#17828 = DIRECTION ( 'NONE',  ( -0.7071067811865492381, 8.659560562354955045E-17, 0.7071067811865457964 ) ) ;
#17829 = PRODUCT_DEFINITION_SHAPE ( 'NONE', 'NONE',  #24107 ) ;
#17830 =( BOUNDED_CURVE ( )  B_SPLINE_CURVE ( 2, ( #13509, #19118, #22434, #3871, #13622, #20957, #11276, #11540, #4240, #18879, #16917 ),
 .UNSPECIFIED., .F., .T. ) 
 B_SPLINE_CURVE_WITH_KNOTS ( ( 3, 2, 2, 2, 2, 3 ),
 ( 0.4000000000000000222, 0.4199999999999999845, 0.4400000000000000022, 0.4599999999999999645, 0.4799999999999999267, 0.4999999999999999445 ),
 .UNSPECIFIED. ) 
 CURVE ( )  GEOMETRIC_REPRESENTATION_ITEM ( )  RATIONAL_B_SPLINE_CURVE ( ( 1.000000000000000000, 0.9510565162951535312, 1.000000000000000000, 0.9510565162951535312, 1.000000000000000000, 0.9510565162951535312, 1.000000000000000000, 0.9510565162951535312, 1.000000000000000000, 0.9510565162951536422, 0.9999999999999998890 ) ) 
 REPRESENTATION_ITEM ( '' )  );
#17831 = ORIENTED_EDGE ( 'NONE', *, *, #19994, .F. ) ;
#17832 = ORIENTED_EDGE ( 'NONE', *, *, #1289, .T. ) ;
#17833 = DIRECTION ( 'NONE',  ( -1.000000000000000000, -0.000000000000000000, -0.000000000000000000 ) ) ;
#17834 = CARTESIAN_POINT ( 'NONE',  ( -7.685661446562381371, 5.583959896777970222, 10.85958914175814449 ) ) ;
#17835 = FACE_OUTER_BOUND ( 'NONE', #7351, .T. ) ;
#17836 = CARTESIAN_POINT ( 'NONE',  ( 33.99999999999998579, 3.999999999999985345, 10.49999999999999822 ) ) ;
#17837 = CARTESIAN_POINT ( 'NONE',  ( 89.12522638709219791, 5.000000000000015987, 0.000000000000000000 ) ) ;
#17838 = VERTEX_POINT ( 'NONE', #10415 ) ;
#17839 = DIRECTION ( 'NONE',  ( 1.000000000000000000, 1.224606353822377258E-16, 0.000000000000000000 ) ) ;
#17840 = EDGE_LOOP ( 'NONE', ( #21612, #3468, #444, #5545 ) ) ;
#17841 = EDGE_CURVE ( 'NONE', #1240, #21393, #12222, .T. ) ;
#17842 = FACE_OUTER_BOUND ( 'NONE', #17170, .T. ) ;
#17843 = ORIENTED_EDGE ( 'NONE', *, *, #20615, .T. ) ;
#17844 = LINE ( 'NONE', #16349, #11353 ) ;
#17845 = CARTESIAN_POINT ( 'NONE',  ( 59.45454545454545325, 7.491529369508391930E-15, 0.000000000000000000 ) ) ;
#17846 = DIRECTION ( 'NONE',  ( 1.000000000000000000, 0.000000000000000000, 0.000000000000000000 ) ) ;
#17847 = EDGE_CURVE ( 'NONE', #21048, #7050, #9877, .T. ) ;
#17848 = DIRECTION ( 'NONE',  ( -1.000000000000000000, -0.000000000000000000, 0.000000000000000000 ) ) ;
#17849 = EDGE_CURVE ( 'NONE', #8542, #16244, #23169, .T. ) ;
#17850 = VERTEX_POINT ( 'NONE', #14187 ) ;
#17851 = EDGE_LOOP ( 'NONE', ( #15116, #12707, #13706, #15625 ) ) ;
#17852 = FACE_OUTER_BOUND ( 'NONE', #14014, .T. ) ;
#17853 = AXIS2_PLACEMENT_3D ( 'NONE', #21761, #5400, #9037 ) ;
#17854 = CIRCLE ( 'NONE', #7317, 5.000000000000007994 ) ;
#17855 = CARTESIAN_POINT ( 'NONE',  ( 2.935661446562616295, -9.035036904803758873, -6.806742014460233747 ) ) ;
#17856 = VERTEX_POINT ( 'NONE', #8821 ) ;
#17857 = ORIENTED_EDGE ( 'NONE', *, *, #11836, .T. ) ;
#17858 = CARTESIAN_POINT ( 'NONE',  ( -3.213650742982549602, -8.577201891241250209, -12.34882418652165548 ) ) ;
#17859 = EDGE_LOOP ( 'NONE', ( #12589, #21181, #19624, #23602 ) ) ;
#17860 = CARTESIAN_POINT ( 'NONE',  ( -31.74999999999995737, 0.000000000000000000, 5.000000000000000888 ) ) ;
#17861 = ORIENTED_EDGE ( 'NONE', *, *, #15026, .F. ) ;
#17862 = DIRECTION ( 'NONE',  ( -1.000000000000000000, -1.224606353822377258E-16, -0.000000000000000000 ) ) ;
#17863 = CARTESIAN_POINT ( 'NONE',  ( 33.99999999999998579, -4.000000000000013323, 10.49999999999999822 ) ) ;
#17864 = CARTESIAN_POINT ( 'NONE',  ( 40.89823313241237912, 26.41789760203348081, 27.00000000000000000 ) ) ;
#17865 = LINE ( 'NONE', #1154, #18074 ) ;
#17866 = ADVANCED_FACE ( 'NONE', ( #7106 ), #11831, .T. ) ;
#17867 = CARTESIAN_POINT ( 'NONE',  ( -30.44534269664590553, -40.40463133211081015, 0.000000000000000000 ) ) ;
#17868 = ORIENTED_EDGE ( 'NONE', *, *, #8108, .F. ) ;
#17869 = CARTESIAN_POINT ( 'NONE',  ( 23.90000000000000568, 29.50000000000000000, 27.00000000000000000 ) ) ;
#17870 = FACE_OUTER_BOUND ( 'NONE', #20397, .T. ) ;
#17871 = LINE ( 'NONE', #6891, #9184 ) ;
#17872 = ORIENTED_EDGE ( 'NONE', *, *, #17876, .F. ) ;
#17873 = VECTOR ( 'NONE', #2016, 1000.000000000000000 ) ;
#17874 = CARTESIAN_POINT ( 'NONE',  ( -5.871322893124554021, 8.081182679343978492, 6.759589141758143072 ) ) ;
#17875 = AXIS2_PLACEMENT_3D ( 'NONE', #8922, #1615, #12711 ) ;
#17876 = EDGE_CURVE ( 'NONE', #8084, #19085, #22952, .T. ) ;
#17877 = EDGE_CURVE ( 'NONE', #1091, #747, #18337, .T. ) ;
#17878 = ORIENTED_EDGE ( 'NONE', *, *, #9604, .T. ) ;
#17879 = ORIENTED_EDGE ( 'NONE', *, *, #19788, .T. ) ;
#17880 = ORIENTED_EDGE ( 'NONE', *, *, #14221, .T. ) ;
#17881 = DIRECTION ( 'NONE',  ( -0.000000000000000000, -0.000000000000000000, 1.000000000000000000 ) ) ;
#17882 = CARTESIAN_POINT ( 'NONE',  ( -14.98950073861089294, -0.6491375924673344899, -9.483449329262338523 ) ) ;
#17883 = CARTESIAN_POINT ( 'NONE',  ( -14.99999999999999645, 15.50000000000000178, 14.70000000000000284 ) ) ;
#17884 = CARTESIAN_POINT ( 'NONE',  ( 0.000000000000000000, 0.000000000000000000, 2.500000000000000000 ) ) ;
#17885 = DIRECTION ( 'NONE',  ( 1.000000000000000000, 0.000000000000000000, 0.000000000000000000 ) ) ;
#17886 = VERTEX_POINT ( 'NONE', #1515 ) ;
#17887 = DIRECTION ( 'NONE',  ( 0.000000000000000000, 0.000000000000000000, 1.000000000000000000 ) ) ;
#17888 = CONICAL_SURFACE ( 'NONE', #17483, 9.500000000000000000, 0.7853981633974500554 ) ;
#17889 = CARTESIAN_POINT ( 'NONE',  ( 5.871322893124551356, -8.081182679343980269, 7.759589141758143072 ) ) ;
#17890 = DIRECTION ( 'NONE',  ( -1.000000000000000000, -0.000000000000000000, 0.000000000000000000 ) ) ;
#17891 = EDGE_CURVE ( 'NONE', #9763, #22408, #7543, .T. ) ;
#17892 = DIRECTION ( 'NONE',  ( 0.7071067811865474617, 8.659560562354932858E-17, -0.7071067811865474617 ) ) ;
#17893 = FACE_OUTER_BOUND ( 'NONE', #12397, .T. ) ;
#17894 = CARTESIAN_POINT ( 'NONE',  ( 76.32931906745326955, 5.000000000000007105, 6.123233995736765296E-16 ) ) ;
#17895 = CARTESIAN_POINT ( 'NONE',  ( 16.18147534945000032, -6.260849737139246862, -7.148624562014513906 ) ) ;
#17896 = DIRECTION ( 'NONE',  ( -1.000000000000000000, -1.224606353822377258E-16, -0.000000000000000000 ) ) ;
#17897 = ADVANCED_FACE ( 'NONE', ( #23826 ), #2105, .T. ) ;
#17898 = CARTESIAN_POINT ( 'NONE',  ( -5.365059087798940141, -7.384370330707086261, -3.933165578109187877 ) ) ;
#17899 = CLOSED_SHELL ( 'NONE', ( #6884, #19018, #5304, #4608, #21992, #14321, #11503, #12728, #14249, #23287, #22668, #13189, #4577, #17075, #9784, #13691, #12058, #5605, #19358, #2428, #17464, #7370, #18332, #23610, #3724, #14716, #23339, #22803 ) ) ;
#17900 = VERTEX_POINT ( 'NONE', #13301 ) ;
#17901 = CARTESIAN_POINT ( 'NONE',  ( 23.00000000000000000, 11.58003564732003277, 1.573866785045813899 ) ) ;
#17902 = VERTEX_POINT ( 'NONE', #20540 ) ;
#17903 = EDGE_CURVE ( 'NONE', #15397, #1786, #7443, .T. ) ;
#17904 = EDGE_CURVE ( 'NONE', #18469, #1139, #5241, .T. ) ;
#17905 = ORIENTED_EDGE ( 'NONE', *, *, #22266, .F. ) ;
#17906 =( LENGTH_UNIT ( ) NAMED_UNIT ( * ) SI_UNIT ( .MILLI., .METRE. ) );
#17907 = DIRECTION ( 'NONE',  ( -0.000000000000000000, 0.000000000000000000, 1.000000000000000000 ) ) ;
#17908 = ORIENTED_EDGE ( 'NONE', *, *, #1857, .T. ) ;
#17909 = ORIENTED_EDGE ( 'NONE', *, *, #15552, .T. ) ;
#17910 = DIRECTION ( 'NONE',  ( -0.000000000000000000, -0.000000000000000000, 1.000000000000000000 ) ) ;
#17911 = CARTESIAN_POINT ( 'NONE',  ( 7.685661446561619314, 5.583959896779020049, -8.259589141758144848 ) ) ;
#17912 = CARTESIAN_POINT ( 'NONE',  ( 23.00000000000000000, 0.000000000000000000, 0.000000000000000000 ) ) ;
#17913 = LINE ( 'NONE', #20222, #16600 ) ;
#17914 = CARTESIAN_POINT ( 'NONE',  ( 23.00000000000000000, 5.823083658124882156, -12.96521604808343398 ) ) ;
#17915 = VECTOR ( 'NONE', #3768, 1000.000000000000000 ) ;
#17916 = SPHERICAL_SURFACE ( 'NONE', #21928, 1.500000000000000000 ) ;
#17917 = CIRCLE ( 'NONE', #9313, 1.000000000000000000 ) ;
#17918 = CARTESIAN_POINT ( 'NONE',  ( 0.000000000000000000, 0.000000000000000000, 0.000000000000000000 ) ) ;
#17919 = EDGE_CURVE ( 'NONE', #22424, #4863, #9172, .T. ) ;
#17920 = ORIENTED_EDGE ( 'NONE', *, *, #4398, .F. ) ;
#17921 = CARTESIAN_POINT ( 'NONE',  ( 23.85000000000000142, 15.03999999999999737, 0.000000000000000000 ) ) ;
#17922 = ORIENTED_EDGE ( 'NONE', *, *, #712, .T. ) ;
#17923 = DIRECTION ( 'NONE',  ( -0.8571673007021116675, 0.000000000000000000, -0.5150380749100552658 ) ) ;
#17924 = CARTESIAN_POINT ( 'NONE',  ( 50.00005079999999680, 1.102182119232617714E-15, -9.000000000000000000 ) ) ;
#17925 = DIRECTION ( 'NONE',  ( -0.000000000000000000, 1.000000000000000000, 1.224646799147353207E-16 ) ) ;
#17926 = EDGE_CURVE ( 'NONE', #19039, #6856, #14895, .T. ) ;
#17927 = ORIENTED_EDGE ( 'NONE', *, *, #10940, .T. ) ;
#17928 = CARTESIAN_POINT ( 'NONE',  ( -8.680847955711200825, 2.820578480813073607, -3.533165578109187965 ) ) ;
#17929 = ORIENTED_EDGE ( 'NONE', *, *, #370, .T. ) ;
#17930 = ORIENTED_EDGE ( 'NONE', *, *, #15507, .F. ) ;
#17931 = CARTESIAN_POINT ( 'NONE',  ( -6.153822176767817416E-13, 9.500000000000000000, 2.559589141758142450 ) ) ;
#17932 = CARTESIAN_POINT ( 'NONE',  ( -6.822232771736903637E-13, 9.988891130263535700, 7.706742014460232326 ) ) ;
#17933 = CARTESIAN_POINT ( 'NONE',  ( 50.00005079999999680, 0.000000000000000000, 0.000000000000000000 ) ) ;
#17934 = ORIENTED_EDGE ( 'NONE', *, *, #20066, .F. ) ;
#17935 = VECTOR ( 'NONE', #4983, 1000.000000000000000 ) ;
#17936 =( NAMED_UNIT ( * ) PLANE_ANGLE_UNIT ( ) SI_UNIT ( $, .RADIAN. ) );
#17937 = VECTOR ( 'NONE', #23449, 1000.000000000000000 ) ;
#17938 = CARTESIAN_POINT ( 'NONE',  ( 41.73082370883258108, -27.62204025492843940, -1.500000000000000000 ) ) ;
#17939 = DIRECTION ( 'NONE',  ( 0.000000000000000000, -1.000000000000000000, 0.000000000000000000 ) ) ;
#17940 = DIRECTION ( 'NONE',  ( 0.000000000000000000, 0.000000000000000000, 1.000000000000000000 ) ) ;
#17941 = FACE_OUTER_BOUND ( 'NONE', #4330, .T. ) ;
#17942 = ORIENTED_EDGE ( 'NONE', *, *, #3764, .T. ) ;
#17943 = LINE ( 'NONE', #6718, #15634 ) ;
#17944 = VERTEX_POINT ( 'NONE', #7568 ) ;
#17945 = DIRECTION ( 'NONE',  ( -1.000000000000000000, 0.000000000000000000, 0.000000000000000000 ) ) ;
#17946 = CARTESIAN_POINT ( 'NONE',  ( -41.49999999999999289, 27.79189783386526358, -27.00000000000000000 ) ) ;
#17947 = CARTESIAN_POINT ( 'NONE',  ( -39.00000000000000711, 29.49999999999999645, 11.00000000000000000 ) ) ;
#17948 = DIRECTION ( 'NONE',  ( 1.000000000000000000, 0.000000000000000000, 0.000000000000000000 ) ) ;
#17949 = AXIS2_PLACEMENT_3D ( 'NONE', #13939, #646, #15757 ) ;
#17950 = DIRECTION ( 'NONE',  ( -0.000000000000000000, -0.000000000000000000, -1.000000000000000000 ) ) ;
#17951 = ADVANCED_FACE ( 'NONE', ( #7801, #17090 ), #4056, .T. ) ;
#17952 = ORIENTED_EDGE ( 'NONE', *, *, #3237, .F. ) ;
#17953 = ADVANCED_FACE ( 'NONE', ( #15014 ), #11107, .T. ) ;
#17954 = DIRECTION ( 'NONE',  ( -0.000000000000000000, 0.000000000000000000, 1.000000000000000000 ) ) ;
#17955 = VERTEX_POINT ( 'NONE', #16974 ) ;
#17956 = CARTESIAN_POINT ( 'NONE',  ( -9.500000000000000000, -6.482511860946779655E-13, -8.206742014460234103 ) ) ;
#17957 = ORIENTED_EDGE ( 'NONE', *, *, #4388, .F. ) ;
#17958 = CARTESIAN_POINT ( 'NONE',  ( 0.000000000000000000, -45.00000000000000000, 0.000000000000000000 ) ) ;
#17959 = VERTEX_POINT ( 'NONE', #11468 ) ;
#17960 = LINE ( 'NONE', #5388, #2217 ) ;
#17961 = CARTESIAN_POINT ( 'NONE',  ( 9.500000000000000000, 1.163414459189985485E-15, 12.50000000000000000 ) ) ;
#17962 = DIRECTION ( 'NONE',  ( -1.000000000000000000, -0.000000000000000000, -0.000000000000000000 ) ) ;
#17964 = ORIENTED_EDGE ( 'NONE', *, *, #9085, .T. ) ;
#17963 = MECHANICAL_DESIGN_GEOMETRIC_PRESENTATION_REPRESENTATION (  '', ( #13665 ), #22248 ) ;
#17965 = DIRECTION ( 'NONE',  ( 0.000000000000000000, 0.9096319953545193293, -0.4154150130018842701 ) ) ;
#17966 = EDGE_CURVE ( 'NONE', #702, #16244, #6664, .T. ) ;
#17967 = CARTESIAN_POINT ( 'NONE',  ( -5.871322893124554021, 8.081182679343978492, -7.906742014460233392 ) ) ;
#17968 = ORIENTED_EDGE ( 'NONE', *, *, #15086, .T. ) ;
#17969 = VERTEX_POINT ( 'NONE', #1746 ) ;
#17970 = CARTESIAN_POINT ( 'NONE',  ( 86.21613547800127719, 7.562528597612068045E-15, 0.000000000000000000 ) ) ;
#17971 = DIRECTION ( 'NONE',  ( 0.000000000000000000, 0.000000000000000000, 1.000000000000000000 ) ) ;
#17972 = CARTESIAN_POINT ( 'NONE',  ( -20.85000000000000142, -15.03999999999999915, -25.00000000000000000 ) ) ;
#17973 = ADVANCED_FACE ( 'NONE', ( #9644 ), #3811, .F. ) ;
#17974 = EDGE_CURVE ( 'NONE', #5826, #9925, #18694, .T. ) ;
#17975 = EDGE_LOOP ( 'NONE', ( #16320, #16297, #1723, #21983 ) ) ;
#17976 = ADVANCED_FACE ( 'NONE', ( #3924 ), #1965, .F. ) ;
#17977 = ADVANCED_FACE ( 'NONE', ( #13185 ), #394, .T. ) ;
#17978 = DIRECTION ( 'NONE',  ( -0.4011779117250717785, -0.9160001545545232160, 0.000000000000000000 ) ) ;
#17979 = DIRECTION ( 'NONE',  ( -1.000000000000000000, -1.224606353822377258E-16, -0.000000000000000000 ) ) ;
#17980 = CARTESIAN_POINT ( 'NONE',  ( 2.454813078130514813E-15, 16.67999999999999972, 13.50000000000000178 ) ) ;
#17981 = AXIS2_PLACEMENT_3D ( 'NONE', #23566, #4779, #11951 ) ;
#17982 = ORIENTED_EDGE ( 'NONE', *, *, #9727, .F. ) ;
#17983 = LINE ( 'NONE', #14544, #18867 ) ;
#17984 = DIRECTION ( 'NONE',  ( -1.000000000000000000, 0.000000000000000000, 0.000000000000000000 ) ) ;
#17985 = DIRECTION ( 'NONE',  ( 0.8571673007021116675, 1.049727191138617833E-16, -0.5150380749100552658 ) ) ;
#17986 = CIRCLE ( 'NONE', #7430, 8.000000000000000000 ) ;
#17987 = CARTESIAN_POINT ( 'NONE',  ( -7.685661446562381371, 5.583959896777970222, 2.859589141758144493 ) ) ;
#17988 = ORIENTED_EDGE ( 'NONE', *, *, #4288, .T. ) ;
#17989 = DIRECTION ( 'NONE',  ( -1.000000000000000000, 0.000000000000000000, 0.000000000000000000 ) ) ;
#17990 = CARTESIAN_POINT ( 'NONE',  ( 7.000000000000000000, 14.02592346138681378, 0.000000000000000000 ) ) ;
#17991 = ADVANCED_FACE ( 'NONE', ( #15243 ), #5861, .F. ) ;
#17992 = DIRECTION ( 'NONE',  ( -1.000000000000000000, 0.000000000000000000, 0.000000000000000000 ) ) ;
#17993 = ORIENTED_EDGE ( 'NONE', *, *, #9451, .T. ) ;
#17994 = CARTESIAN_POINT ( 'NONE',  ( -17.38971744193259994, -8.915620082851749117, -3.315798060087244981 ) ) ;
#17995 = VECTOR ( 'NONE', #20823, 1000.000000000000000 ) ;
#17996 = DIRECTION ( 'NONE',  ( 0.000000000000000000, -0.2817325568414367765, 0.9594929736144953702 ) ) ;
#17997 = ORIENTED_EDGE ( 'NONE', *, *, #7026, .T. ) ;
#17998 = CARTESIAN_POINT ( 'NONE',  ( 0.9999999999999986677, 0.000000000000000000, 0.000000000000000000 ) ) ;
#17999 = CARTESIAN_POINT ( 'NONE',  ( 40.23082370883260239, 29.49999999999999645, -3.000000000000000000 ) ) ;
#18000 = CARTESIAN_POINT ( 'NONE',  ( -7.685661446562381371, 5.583959896777970222, 4.006742014460233925 ) ) ;
#18001 = EDGE_CURVE ( 'NONE', #23971, #12836, #5649, .T. ) ;
#18002 = CYLINDRICAL_SURFACE ( 'NONE', #19867, 17.87500000001787726 ) ;
#18003 = EDGE_CURVE ( 'NONE', #2256, #14909, #288, .T. ) ;
#18004 = CARTESIAN_POINT ( 'NONE',  ( 30.44534269664590909, -40.40463133211080304, -27.00000000000000000 ) ) ;
#18005 = CARTESIAN_POINT ( 'NONE',  ( 15.57833309066359817, -5.219313726039669810, -7.987432870209351776 ) ) ;
#18006 = DIRECTION ( 'NONE',  ( -1.000000000000000000, 0.000000000000000000, 0.000000000000000000 ) ) ;
#18007 = CARTESIAN_POINT ( 'NONE',  ( -31.10231664966676846, -45.36128193761570770, 12.00000000000000000 ) ) ;
#18008 = ORIENTED_EDGE ( 'NONE', *, *, #23393, .F. ) ;
#18009 = DIRECTION ( 'NONE',  ( 0.7071067811865660024, 8.659560562355159656E-17, -0.7071067811865291430 ) ) ;
#18010 = ORIENTED_EDGE ( 'NONE', *, *, #3499, .F. ) ;
#18011 = AXIS2_PLACEMENT_3D ( 'NONE', #22069, #12769, #10568 ) ;
#18012 = AXIS2_PLACEMENT_3D ( 'NONE', #2549, #15575, #17299 ) ;
#18013 = AXIS2_PLACEMENT_3D ( 'NONE', #16311, #8394, #23307 ) ;
#18014 = PRODUCT_DEFINITION_SHAPE ( 'NONE', 'NONE',  #24104 ) ;
#18015 = AXIS2_PLACEMENT_3D ( 'NONE', #17863, #21518, #21646 ) ;
#18016 = DIRECTION ( 'NONE',  ( -0.9999999999999998890, 0.000000000000000000, 0.000000000000000000 ) ) ;
#18017 = VECTOR ( 'NONE', #4942, 1000.000000000000000 ) ;
#18018 = LINE ( 'NONE', #14341, #10505 ) ;
#18019 = ORIENTED_EDGE ( 'NONE', *, *, #18473, .T. ) ;
#18020 = CARTESIAN_POINT ( 'NONE',  ( 41.00000000000000000, -6.000000000000015099, 10.49999999999999822 ) ) ;
#18021 = CARTESIAN_POINT ( 'NONE',  ( -5.871322893124554021, 8.081182679343978492, -8.759589141758141295 ) ) ;
#18022 = LINE ( 'NONE', #1318, #9880 ) ;
#18023 = DIRECTION ( 'NONE',  ( -1.000000000000000000, 0.000000000000000000, 0.000000000000000000 ) ) ;
#18024 = CARTESIAN_POINT ( 'NONE',  ( -6.153822176767817416E-13, 9.500000000000000000, 3.706742014460231882 ) ) ;
#18025 = DIRECTION ( 'NONE',  ( 1.000000000000000000, 0.000000000000000000, 0.000000000000000000 ) ) ;
#18026 = EDGE_LOOP ( 'NONE', ( #20226, #17997, #9534 ) ) ;
#18027 = DIRECTION ( 'NONE',  ( -0.000000000000000000, -0.000000000000000000, -1.000000000000000000 ) ) ;
#18028 = VECTOR ( 'NONE', #11155, 1000.000000000000000 ) ;
#18029 = CIRCLE ( 'NONE', #13321, 20.85000000000000142 ) ;
#18030 = CARTESIAN_POINT ( 'NONE',  ( 74.87477361290781630, 7.420530141404717394E-15, 0.000000000000000000 ) ) ;
#18031 = AXIS2_PLACEMENT_3D ( 'NONE', #9010, #23916, #7191 ) ;
#18032 = LINE ( 'NONE', #1332, #14121 ) ;
#18033 = EDGE_CURVE ( 'NONE', #1413, #2386, #21468, .T. ) ;
#18034 = PLANE ( 'NONE',  #19192 ) ;
#18035 = AXIS2_PLACEMENT_3D ( 'NONE', #5247, #20250, #3773 ) ;
#18036 = DIRECTION ( 'NONE',  ( 1.000000000000000000, 0.000000000000000000, 0.000000000000000000 ) ) ;
#18037 = DIRECTION ( 'NONE',  ( 0.000000000000000000, 0.000000000000000000, 1.000000000000000000 ) ) ;
#18038 = VECTOR ( 'NONE', #11324, 1000.000000000000000 ) ;
#18039 = AXIS2_PLACEMENT_3D ( 'NONE', #20634, #9511, #501 ) ;
#18040 = DIRECTION ( 'NONE',  ( 0.8571673007021116675, 1.049727191138617833E-16, -0.5150380749100552658 ) ) ;
#18041 = ORIENTED_EDGE ( 'NONE', *, *, #16556, .T. ) ;
#18042 = CARTESIAN_POINT ( 'NONE',  ( 86.51113724927145654, -9.244463733058732095E-30, 5.000000000000007994 ) ) ;
#18043 = VECTOR ( 'NONE', #1503, 1000.000000000000000 ) ;
#18044 = ORIENTED_EDGE ( 'NONE', *, *, #11214, .T. ) ;
#18045 = ORIENTED_EDGE ( 'NONE', *, *, #17794, .F. ) ;
#18046 = CARTESIAN_POINT ( 'NONE',  ( 6.809999908187194197E-13, -9.988891130263535700, 12.70674201446023410 ) ) ;
#18047 = DIRECTION ( 'NONE',  ( -0.000000000000000000, -1.000000000000000000, -0.000000000000000000 ) ) ;
#18048 = EDGE_LOOP ( 'NONE', ( #20963, #6405, #3846, #634 ) ) ;
#18049 = DIRECTION ( 'NONE',  ( -0.9160001545545232160, -0.4011779117250717785, 0.000000000000000000 ) ) ;
#18050 = VECTOR ( 'NONE', #7126, 1000.000000000000000 ) ;
#18051 = AXIS2_PLACEMENT_3D ( 'NONE', #5761, #13176, #4547 ) ;
#18052 = CARTESIAN_POINT ( 'NONE',  ( -31.74999999999995737, 6.123233995736767268E-16, -5.000000000000000888 ) ) ;
#18053 = DIRECTION ( 'NONE',  ( 0.000000000000000000, 0.000000000000000000, 1.000000000000000000 ) ) ;
#18054 = EDGE_CURVE ( 'NONE', #10216, #1666, #2594, .T. ) ;
#18055 = CIRCLE ( 'NONE', #1680, 4.999999999999997335 ) ;
#18056 = VECTOR ( 'NONE', #22399, 1000.000000000000000 ) ;
#18057 = ADVANCED_BREP_SHAPE_REPRESENTATION ( '', ( #10843, #8005 ), #21672 ) ;
#18058 = AXIS2_PLACEMENT_3D ( 'NONE', #22584, #5865, #2082 ) ;
#18059 = DIRECTION ( 'NONE',  ( 1.000000000000000000, 1.224606353822377258E-16, 0.000000000000000000 ) ) ;
#18060 = LINE ( 'NONE', #23561, #5320 ) ;
#18061 = DIRECTION ( 'NONE',  ( -0.000000000000000000, -0.000000000000000000, -1.000000000000000000 ) ) ;
#18062 = ADVANCED_FACE ( 'NONE', ( #17462 ), #2337, .F. ) ;
#18063 = CIRCLE ( 'NONE', #11021, 1.499999999999999556 ) ;
#18064 = ORIENTED_EDGE ( 'NONE', *, *, #10738, .F. ) ;
#18065 = APPLICATION_CONTEXT ( 'automotive_design' ) ;
#18066 = EDGE_CURVE ( 'NONE', #6680, #7419, #761, .T. ) ;
#18067 = EDGE_LOOP ( 'NONE', ( #16905, #17285, #4891, #18974 ) ) ;
#18068 = DIRECTION ( 'NONE',  ( 0.5000000000000001110, -0.8660254037844384856, 0.000000000000000000 ) ) ;
#18069 = CARTESIAN_POINT ( 'NONE',  ( 23.90000000000000568, -29.50000000000000355, 12.00000000000000000 ) ) ;
#18070 = DIRECTION ( 'NONE',  ( -0.000000000000000000, -0.000000000000000000, -1.000000000000000000 ) ) ;
#18071 = CARTESIAN_POINT ( 'NONE',  ( -41.00000000000000000, -6.000000000000000888, 10.49999999999999822 ) ) ;
#18072 = CIRCLE ( 'NONE', #13776, 17.87500000001787726 ) ;
#18073 = DIRECTION ( 'NONE',  ( -1.000000000000000000, 0.000000000000000000, 0.000000000000000000 ) ) ;
#18074 = VECTOR ( 'NONE', #8571, 1000.000000000000000 ) ;
#18075 = DIRECTION ( 'NONE',  ( -0.8571673007021116675, 0.000000000000000000, -0.5150380749100552658 ) ) ;
#18076 = TOROIDAL_SURFACE ( 'NONE', #11416, 12.73082370883260417, 1.500000000000000000 ) ;
#18077 = VERTEX_POINT ( 'NONE', #9887 ) ;
#18078 = CARTESIAN_POINT ( 'NONE',  ( -9.500000000000000000, -6.482511860946779655E-13, -7.059589141758143782 ) ) ;
#18079 = CIRCLE ( 'NONE', #6770, 1.000000000000000888 ) ;
#18080 = EDGE_LOOP ( 'NONE', ( #2310, #9421, #8751, #5358 ) ) ;
#18081 = AXIS2_PLACEMENT_3D ( 'NONE', #23477, #16366, #5289 ) ;
#18082 = FACE_OUTER_BOUND ( 'NONE', #14813, .T. ) ;
#18083 = DIRECTION ( 'NONE',  ( -1.000000000000000000, -1.224606353822377258E-16, -0.000000000000000000 ) ) ;
#18084 = AXIS2_PLACEMENT_3D ( 'NONE', #9932, #15294, #562 ) ;
#18085 = EDGE_LOOP ( 'NONE', ( #7664, #10020, #13368, #22499 ) ) ;
#18086 = LINE ( 'NONE', #11310, #20159 ) ;
#18087 = DIRECTION ( 'NONE',  ( 0.000000000000000000, 0.000000000000000000, 1.000000000000000000 ) ) ;
#18088 = CARTESIAN_POINT ( 'NONE',  ( -2.935661446561384391, -9.035036904804158553, -3.459589141758144137 ) ) ;
#18089 = DIRECTION ( 'NONE',  ( -1.000000000000000000, 0.000000000000000000, 0.000000000000000000 ) ) ;
#18090 = ORIENTED_EDGE ( 'NONE', *, *, #19330, .T. ) ;
#18091 = DIRECTION ( 'NONE',  ( -0.000000000000000000, -0.000000000000000000, 1.000000000000000000 ) ) ;
#18092 = EDGE_CURVE ( 'NONE', #5776, #1413, #6245, .T. ) ;
#18093 = CARTESIAN_POINT ( 'NONE',  ( -41.49999999999999289, -27.79189783386527779, 27.00000000000000000 ) ) ;
#18094 = EDGE_CURVE ( 'NONE', #15532, #8263, #9737, .T. ) ;
#18095 = AXIS2_PLACEMENT_3D ( 'NONE', #15238, #9281, #11590 ) ;
#18096 = CARTESIAN_POINT ( 'NONE',  ( 9.500000000000000000, 6.470877716354879437E-13, -7.206742014460234103 ) ) ;
#18097 = ORIENTED_EDGE ( 'NONE', *, *, #9965, .F. ) ;
#18098 = VECTOR ( 'NONE', #5268, 1000.000000000000000 ) ;
#18099 = DIRECTION ( 'NONE',  ( 1.000000000000000000, 0.000000000000000000, -0.000000000000000000 ) ) ;
#18100 = DIRECTION ( 'NONE',  ( -0.000000000000000000, -0.000000000000000000, -1.000000000000000000 ) ) ;
#18101 = AXIS2_PLACEMENT_3D ( 'NONE', #10636, #6989, #12359 ) ;
#18102 = VECTOR ( 'NONE', #19723, 1000.000000000000000 ) ;
#18103 = DIRECTION ( 'NONE',  ( -0.000000000000000000, -0.000000000000000000, -1.000000000000000000 ) ) ;
#18104 = AXIS2_PLACEMENT_3D ( 'NONE', #12653, #14470, #18167 ) ;
#18105 = ORIENTED_EDGE ( 'NONE', *, *, #20979, .F. ) ;
#18106 = CARTESIAN_POINT ( 'NONE',  ( 9.500000000000209610, -3.086737114211962396, -3.959589141758144581 ) ) ;
#18107 = CARTESIAN_POINT ( 'NONE',  ( 23.00000000000000000, -10.66755332433018744, -4.772587172891147311 ) ) ;
#18108 = VERTEX_POINT ( 'NONE', #21122 ) ;
#18109 = CARTESIAN_POINT ( 'NONE',  ( 7.999999999999986677, 1.040949779275249548E-15, 53.00000000000000000 ) ) ;
#18110 = CYLINDRICAL_SURFACE ( 'NONE', #18416, 18.49999999999999645 ) ;
#18111 = DIRECTION ( 'NONE',  ( -0.000000000000000000, -0.000000000000000000, -1.000000000000000000 ) ) ;
#18112 = CARTESIAN_POINT ( 'NONE',  ( -7.685661446561619314, -5.583959896779019161, 3.259589141758143516 ) ) ;
#18113 =( BOUNDED_CURVE ( )  B_SPLINE_CURVE ( 2, ( #4734, #15565, #12144, #17284, #17788, #13750, #1083, #4505, #15944 ),
 .UNSPECIFIED., .F., .T. ) 
 B_SPLINE_CURVE_WITH_KNOTS ( ( 3, 2, 2, 2, 3 ),
 ( 0.1207052568533188708, 0.1400000000000000133, 0.1600000000000000033, 0.1799999999999999933, 0.2000000000000000111 ),
 .UNSPECIFIED. ) 
 CURVE ( )  GEOMETRIC_REPRESENTATION_ITEM ( )  RATIONAL_B_SPLINE_CURVE ( ( 0.9966699465879109709, 0.9527824026605606900, 1.000000000000000000, 0.9510565162951535312, 1.000000000000000000, 0.9510565162951535312, 1.000000000000000000, 0.9510565162951535312, 1.000000000000000000 ) ) 
 REPRESENTATION_ITEM ( '' )  );
#18114 = AXIS2_PLACEMENT_3D ( 'NONE', #574, #7748, #5577 ) ;
#18115 = ADVANCED_FACE ( 'NONE', ( #1341 ), #16374, .T. ) ;
#18116 = AXIS2_PLACEMENT_3D ( 'NONE', #16707, #5617, #13042 ) ;
#18117 = ORIENTED_EDGE ( 'NONE', *, *, #11273, .T. ) ;
#18118 = VECTOR ( 'NONE', #21554, 1000.000000000000000 ) ;
#18119 = ORIENTED_EDGE ( 'NONE', *, *, #4334, .F. ) ;
#18120 = AXIS2_PLACEMENT_3D ( 'NONE', #6579, #19868, #17537 ) ;
#18121 = ORIENTED_EDGE ( 'NONE', *, *, #11382, .T. ) ;
#18122 = EDGE_CURVE ( 'NONE', #5301, #7700, #19176, .T. ) ;
#18123 = VERTEX_POINT ( 'NONE', #19064 ) ;
#18124 = DIRECTION ( 'NONE',  ( 0.000000000000000000, 0.000000000000000000, 1.000000000000000000 ) ) ;
#18125 = EDGE_CURVE ( 'NONE', #8876, #13479, #18341, .T. ) ;
#18126 = AXIS2_PLACEMENT_3D ( 'NONE', #5332, #16663, #3253 ) ;
#18127 = DIRECTION ( 'NONE',  ( 0.000000000000000000, 0.000000000000000000, 1.000000000000000000 ) ) ;
#18128 = CARTESIAN_POINT ( 'NONE',  ( -31.10231664966676135, 45.36128193761570770, 27.00000000000000000 ) ) ;
#18129 = ORIENTED_EDGE ( 'NONE', *, *, #22889, .F. ) ;
#18130 = ORIENTED_EDGE ( 'NONE', *, *, #14084, .T. ) ;
#18131 = CARTESIAN_POINT ( 'NONE',  ( 9.000000000000001776, 6.130305204967781210E-13, 12.50000000000000000 ) ) ;
#18132 = ORIENTED_EDGE ( 'NONE', *, *, #13645, .F. ) ;
#18133 = CARTESIAN_POINT ( 'NONE',  ( 5.871322893124551356, -8.081182679343980269, -8.906742014460233392 ) ) ;
#18134 = DIRECTION ( 'NONE',  ( 0.000000000000000000, 0.000000000000000000, -1.000000000000000000 ) ) ;
#18135 = DIRECTION ( 'NONE',  ( 0.000000000000000000, 0.000000000000000000, 1.000000000000000000 ) ) ;
#18136 = LINE ( 'NONE', #1429, #21813 ) ;
#18137 = DIRECTION ( 'NONE',  ( -0.000000000000000000, -0.000000000000000000, 1.000000000000000000 ) ) ;
#18138 = DIRECTION ( 'NONE',  ( -0.000000000000000000, -0.000000000000000000, -1.000000000000000000 ) ) ;
#18139 = DIRECTION ( 'NONE',  ( -0.1039766011667100087, 0.9945797436152714610, 0.000000000000000000 ) ) ;
#18140 = CARTESIAN_POINT ( 'NONE',  ( -5.365059087799948223, 7.384370330706355290, -3.333165578109187344 ) ) ;
#18141 = ORIENTED_EDGE ( 'NONE', *, *, #6049, .F. ) ;
#18142 = CARTESIAN_POINT ( 'NONE',  ( -2.682529543900285862, 8.255977015246234174, 9.233165578109188587 ) ) ;
#18143 = EDGE_CURVE ( 'NONE', #11511, #16661, #21845, .T. ) ;
#18144 = EDGE_LOOP ( 'NONE', ( #545, #2229, #18964, #11049 ) ) ;
#18145 = APPLICATION_PROTOCOL_DEFINITION ( 'draft international standard', 'automotive_design', 1998, #4014 ) ;
#18146 = EDGE_CURVE ( 'NONE', #21867, #21197, #20292, .T. ) ;
#18147 = PLANE ( 'NONE',  #10875 ) ;
#18148 = ORIENTED_EDGE ( 'NONE', *, *, #8013, .T. ) ;
#18149 = ORIENTED_EDGE ( 'NONE', *, *, #23260, .F. ) ;
#18150 = EDGE_CURVE ( 'NONE', #19513, #11923, #14421, .T. ) ;
#18151 = DIRECTION ( 'NONE',  ( 1.000000000000000000, 0.000000000000000000, 0.000000000000000000 ) ) ;
#18152 = CARTESIAN_POINT ( 'NONE',  ( -2.935661446561384391, -9.035036904804158553, -7.459589141758144137 ) ) ;
#18153 = EDGE_CURVE ( 'NONE', #1347, #9461, #8578, .T. ) ;
#18154 = CIRCLE ( 'NONE', #21268, 5.000000000000007994 ) ;
#18155 = CARTESIAN_POINT ( 'NONE',  ( 2.693686482235166046, 8.587799726479698137, 100.3350131173703659 ) ) ;
#18156 = LINE ( 'NONE', #10908, #23243 ) ;
#18157 = CARTESIAN_POINT ( 'NONE',  ( 40.00000000000000000, -29.50000000000000000, -27.00000000000000000 ) ) ;
#18158 = AXIS2_PLACEMENT_3D ( 'NONE', #9201, #16650, #24087 ) ;
#18159 = DIRECTION ( 'NONE',  ( -1.000000000000000000, -0.000000000000000000, -0.000000000000000000 ) ) ;
#18160 = CONICAL_SURFACE ( 'NONE', #20504, 4.172000000000008590, 0.9599310885968742602 ) ;
#18161 = DIRECTION ( 'NONE',  ( -1.000000000000000000, 0.000000000000000000, 0.000000000000000000 ) ) ;
#18162 = EDGE_LOOP ( 'NONE', ( #11547, #14432 ) ) ;
#18163 = EDGE_LOOP ( 'NONE', ( #21472, #12349, #17135, #4124 ) ) ;
#18164 = CARTESIAN_POINT ( 'NONE',  ( 23.00000000000000000, 17.02535186363804698, 5.445458559199168214 ) ) ;
#18165 = CARTESIAN_POINT ( 'NONE',  ( 87.09090909090909349, 4.172000000000015696, 5.109226446042767468E-16 ) ) ;
#18166 = CARTESIAN_POINT ( 'NONE',  ( 17.57831567727901145, 9.462949834988604536, -0.9681625741885153680 ) ) ;
#18167 = DIRECTION ( 'NONE',  ( -1.000000000000000000, 0.000000000000000000, 0.000000000000000000 ) ) ;
#18168 = ORIENTED_EDGE ( 'NONE', *, *, #22771, .F. ) ;
#18169 = LINE ( 'NONE', #5349, #22322 ) ;
#18170 = CARTESIAN_POINT ( 'NONE',  ( 9.499999999999790390, 3.086737114213260025, -9.306742014460233747 ) ) ;
#18171 = VECTOR ( 'NONE', #13122, 1000.000000000000227 ) ;
#18172 = AXIS2_PLACEMENT_3D ( 'NONE', #16222, #23431, #23902 ) ;
#18173 = FACE_OUTER_BOUND ( 'NONE', #6843, .T. ) ;
#18174 = ORIENTED_EDGE ( 'NONE', *, *, #5638, .F. ) ;
#18175 = CIRCLE ( 'NONE', #22838, 23.85000000000000142 ) ;
#18176 = ORIENTED_EDGE ( 'NONE', *, *, #4260, .T. ) ;
#18177 = CARTESIAN_POINT ( 'NONE',  ( 6.809999908187194197E-13, -9.988891130263535700, 5.559589141758142894 ) ) ;
#18178 = CARTESIAN_POINT ( 'NONE',  ( -2.935661446561384391, -9.035036904804158553, 8.606742014460234458 ) ) ;
#18179 = DIRECTION ( 'NONE',  ( -0.7071067811865457964, 0.000000000000000000, -0.7071067811865492381 ) ) ;
#18180 = ORIENTED_EDGE ( 'NONE', *, *, #817, .T. ) ;
#18181 = ORIENTED_EDGE ( 'NONE', *, *, #1929, .T. ) ;
#18182 = AXIS2_PLACEMENT_3D ( 'NONE', #17933, #1221, #10926 ) ;
#18183 = CIRCLE ( 'NONE', #8427, 1.000000000000000888 ) ;
#18184 = CYLINDRICAL_SURFACE ( 'NONE', #10576, 11.23082370883260417 ) ;
#18185 = FACE_OUTER_BOUND ( 'NONE', #15965, .T. ) ;
#18186 = CARTESIAN_POINT ( 'NONE',  ( -7.685661446561619314, -5.583959896779019161, 3.259589141758143516 ) ) ;
#18187 = CARTESIAN_POINT ( 'NONE',  ( 1.016919733032271456, 45.00000000000000000, 0.000000000000000000 ) ) ;
#18188 = ADVANCED_FACE ( 'NONE', ( #11962 ), #17344, .T. ) ;
#18189 = EDGE_CURVE ( 'NONE', #4544, #11455, #9750, .T. ) ;
#18190 = FACE_OUTER_BOUND ( 'NONE', #15044, .T. ) ;
#18191 = CARTESIAN_POINT ( 'NONE',  ( 12.50000000000000178, 5.755434930044642846E-15, -2.500000000000000000 ) ) ;
#18192 = AXIS2_PLACEMENT_3D ( 'NONE', #13725, #15665, #6420 ) ;
#18193 = ORIENTED_EDGE ( 'NONE', *, *, #15206, .T. ) ;
#18194 = AXIS2_PLACEMENT_3D ( 'NONE', #2537, #13521, #15695 ) ;
#18195 = CYLINDRICAL_SURFACE ( 'NONE', #19139, 9.500000000000000000 ) ;
#18196 = FACE_BOUND ( 'NONE', #2394, .T. ) ;
#18197 = CARTESIAN_POINT ( 'NONE',  ( -3.342360423240396727, 8.897987090007918098, -3.499485096983522059 ) ) ;
#18198 = DIRECTION ( 'NONE',  ( -0.000000000000000000, -0.000000000000000000, -1.000000000000000000 ) ) ;
#18199 = DIRECTION ( 'NONE',  ( 1.000000000000000000, 0.000000000000000000, 0.000000000000000000 ) ) ;
#18200 = DIRECTION ( 'NONE',  ( -0.000000000000000000, -0.000000000000000000, 1.000000000000000000 ) ) ;
#18201 = ORIENTED_EDGE ( 'NONE', *, *, #8938, .F. ) ;
#18202 = CARTESIAN_POINT ( 'NONE',  ( -9.500000000000211386, 3.086737114211961064, -6.959589141758143249 ) ) ;
#18203 = ORIENTED_EDGE ( 'NONE', *, *, #6648, .F. ) ;
#18204 = EDGE_CURVE ( 'NONE', #12836, #14353, #10128, .T. ) ;
#18205 = CARTESIAN_POINT ( 'NONE',  ( -8.680847955710813579, -2.820578480814257549, 5.733165578109188587 ) ) ;
#18206 = VECTOR ( 'NONE', #6860, 1000.000000000000000 ) ;
#18207 = ORIENTED_EDGE ( 'NONE', *, *, #12702, .F. ) ;
#18208 = DIRECTION ( 'NONE',  ( 1.000000000000000000, 0.000000000000000000, -0.000000000000000000 ) ) ;
#18209 = DIRECTION ( 'NONE',  ( 0.000000000000000000, 0.000000000000000000, 1.000000000000000000 ) ) ;
#18210 = EDGE_CURVE ( 'NONE', #17470, #14876, #11675, .T. ) ;
#18211 = DIRECTION ( 'NONE',  ( 0.000000000000000000, -0.000000000000000000, -1.000000000000000000 ) ) ;
#18212 = EDGE_CURVE ( 'NONE', #8169, #21352, #10906, .T. ) ;
#18213 = VERTEX_POINT ( 'NONE', #17573 ) ;
#18214 = LINE ( 'NONE', #14525, #18043 ) ;
#18215 = DIRECTION ( 'NONE',  ( 0.000000000000000000, -1.000000000000000000, 0.000000000000000000 ) ) ;
#18216 = CARTESIAN_POINT ( 'NONE',  ( 5.871322893124553133, -8.081182679343980269, -11.75958914175814485 ) ) ;
#18217 = ORIENTED_EDGE ( 'NONE', *, *, #9987, .F. ) ;
#18218 = VERTEX_POINT ( 'NONE', #878 ) ;
#18219 = DIRECTION ( 'NONE',  ( -0.000000000000000000, -0.000000000000000000, -1.000000000000000000 ) ) ;
#18220 = CARTESIAN_POINT ( 'NONE',  ( 8.000000000000007105, 0.000000000000000000, 0.000000000000000000 ) ) ;
#18221 = DIRECTION ( 'NONE',  ( -0.000000000000000000, -0.000000000000000000, -1.000000000000000000 ) ) ;
#18222 = ORIENTED_EDGE ( 'NONE', *, *, #3438, .F. ) ;
#18223 = PRODUCT ( 'Drive End Plate', 'Drive End Plate', '', ( #10675 ) ) ;
#18224 = CARTESIAN_POINT ( 'NONE',  ( 9.500000000000000000, 6.470877716354879437E-13, -4.059589141758143782 ) ) ;
#18225 = DIRECTION ( 'NONE',  ( 0.000000000000000000, -1.000000000000000000, 0.000000000000000000 ) ) ;
#18226 = VERTEX_POINT ( 'NONE', #8304 ) ;
#18227 = CARTESIAN_POINT ( 'NONE',  ( -6.153822176767817416E-13, 9.500000000000000000, -3.500000000000014211 ) ) ;
#18228 = EDGE_CURVE ( 'NONE', #18226, #10247, #1198, .T. ) ;
#18229 = CARTESIAN_POINT ( 'NONE',  ( 0.000000000000000000, -15.03999999999999737, 2.200000000000000178 ) ) ;
#18230 = DIRECTION ( 'NONE',  ( -0.000000000000000000, 0.000000000000000000, 1.000000000000000000 ) ) ;
#18231 = DIRECTION ( 'NONE',  ( 0.000000000000000000, -1.000000000000000000, 0.000000000000000000 ) ) ;
#18232 = ORIENTED_EDGE ( 'NONE', *, *, #6799, .T. ) ;
#18233 = AXIS2_PLACEMENT_3D ( 'NONE', #10511, #17971, #14300 ) ;
#18234 = ORIENTED_EDGE ( 'NONE', *, *, #5463, .T. ) ;
#18235 = ORIENTED_EDGE ( 'NONE', *, *, #21415, .T. ) ;
#18236 = DIRECTION ( 'NONE',  ( 0.000000000000000000, 0.000000000000000000, 1.000000000000000000 ) ) ;
#18237 = CARTESIAN_POINT ( 'NONE',  ( 31.10231664966676846, 45.36128193761570770, 11.00000000000000000 ) ) ;
#18238 = ORIENTED_EDGE ( 'NONE', *, *, #7494, .T. ) ;
#18239 = VERTEX_POINT ( 'NONE', #14366 ) ;
#18240 = DIRECTION ( 'NONE',  ( -1.000000000000000000, 0.000000000000000000, 0.000000000000000000 ) ) ;
#18241 = VERTEX_POINT ( 'NONE', #16428 ) ;
#18242 = LINE ( 'NONE', #5426, #20886 ) ;
#18243 = CARTESIAN_POINT ( 'NONE',  ( -34.00000000000000000, -3.851859888774471706E-31, 12.00000000000000000 ) ) ;
#18244 = DIRECTION ( 'NONE',  ( -1.000000000000000000, -0.000000000000000000, -0.000000000000000000 ) ) ;
#18245 = PLANE ( 'NONE',  #14027 ) ;
#18246 = DIRECTION ( 'NONE',  ( -1.000000000000000000, -1.224606353822377258E-16, -0.000000000000000000 ) ) ;
#18247 = AXIS2_PLACEMENT_3D ( 'NONE', #8864, #16304, #22181 ) ;
#18248 = EDGE_CURVE ( 'NONE', #19205, #9146, #12851, .T. ) ;
#18249 = AXIS2_PLACEMENT_3D ( 'NONE', #5672, #3830, #1987 ) ;
#18250 = CARTESIAN_POINT ( 'NONE',  ( 74.87477361290781630, -9.244463733058732095E-30, 5.000000000000007994 ) ) ;
#18251 = EDGE_CURVE ( 'NONE', #16231, #10954, #7044, .T. ) ;
#18252 = CYLINDRICAL_SURFACE ( 'NONE', #1702, 20.85000000000000853 ) ;
#18253 = ADVANCED_FACE ( 'NONE', ( #12656 ), #8881, .F. ) ;
#18254 = CYLINDRICAL_SURFACE ( 'NONE', #15415, 5.000000000000000888 ) ;
#18255 = CARTESIAN_POINT ( 'NONE',  ( 5.365059087798938364, 7.384370330707087149, 10.93316557810918788 ) ) ;
#18256 = MANIFOLD_SOLID_BREP ( 'Mirror1', #9279 ) ;
#18257 = ORIENTED_EDGE ( 'NONE', *, *, #12078, .F. ) ;
#18258 = DIRECTION ( 'NONE',  ( 2.775557561562891351E-17, 0.000000000000000000, -1.000000000000000000 ) ) ;
#18259 = CARTESIAN_POINT ( 'NONE',  ( -28.99999999999999645, -29.50000000000001066, -27.00000000000000000 ) ) ;
#18260 = ORIENTED_EDGE ( 'NONE', *, *, #74, .F. ) ;
#18261 = EDGE_LOOP ( 'NONE', ( #21708, #643, #1544 ) ) ;
#18262 = CARTESIAN_POINT ( 'NONE',  ( -31.50000000000001421, 50.99999999999999289, 12.50000000000000000 ) ) ;
#18263 = CARTESIAN_POINT ( 'NONE',  ( 6.809999908187194197E-13, -9.988891130263535700, -3.559589141758143338 ) ) ;
#18264 = AXIS2_PLACEMENT_3D ( 'NONE', #9512, #22585, #385 ) ;
#18265 = CARTESIAN_POINT ( 'NONE',  ( -30.68762588338046982, -45.64284848299540442, -3.000000000000000000 ) ) ;
#18266 = CARTESIAN_POINT ( 'NONE',  ( 0.2999999999999999334, 0.000000000000000000, 0.000000000000000000 ) ) ;
#18267 = CARTESIAN_POINT ( 'NONE',  ( 6.699999999999996625, 0.000000000000000000, 0.000000000000000000 ) ) ;
#18268 = DIRECTION ( 'NONE',  ( 0.000000000000000000, 0.000000000000000000, -1.000000000000000000 ) ) ;
#18269 = EDGE_LOOP ( 'NONE', ( #13102, #13635, #12071 ) ) ;
#18270 = CARTESIAN_POINT ( 'NONE',  ( 23.00000000000000000, -11.55437235128772500, -1.752358929577761515 ) ) ;
#18271 = ADVANCED_FACE ( 'NONE', ( #6944 ), #22306, .T. ) ;
#18272 = ORIENTED_EDGE ( 'NONE', *, *, #13361, .T. ) ;
#18273 = DIRECTION ( 'NONE',  ( -0.000000000000000000, -0.000000000000000000, 1.000000000000000000 ) ) ;
#18274 = ORIENTED_EDGE ( 'NONE', *, *, #4675, .F. ) ;
#18275 = DIRECTION ( 'NONE',  ( -1.000000000000000000, -1.224606353822377258E-16, -0.000000000000000000 ) ) ;
#18276 = DIRECTION ( 'NONE',  ( -1.000000000000000000, 0.000000000000000000, 0.000000000000000000 ) ) ;
#18277 = DIRECTION ( 'NONE',  ( -1.000000000000000000, -0.000000000000000000, -0.000000000000000000 ) ) ;
#18278 = EDGE_CURVE ( 'NONE', #9714, #6675, #21483, .T. ) ;
#18279 = DIRECTION ( 'NONE',  ( -1.000000000000000000, 0.000000000000000000, 0.000000000000000000 ) ) ;
#18280 = ADVANCED_FACE ( 'NONE', ( #10816 ), #13268, .T. ) ;
#18281 = VERTEX_POINT ( 'NONE', #10701 ) ;
#18282 = DIRECTION ( 'NONE',  ( -0.000000000000000000, 1.000000000000000000, -0.000000000000000000 ) ) ;
#18283 = EDGE_CURVE ( 'NONE', #5821, #21492, #12775, .T. ) ;
#18284 = ADVANCED_FACE ( 'NONE', ( #18173 ), #13014, .T. ) ;
#18285 = DIRECTION ( 'NONE',  ( 1.000000000000000000, 0.000000000000000000, 0.000000000000000000 ) ) ;
#18286 = ORIENTED_EDGE ( 'NONE', *, *, #5896, .T. ) ;
#18287 = VERTEX_POINT ( 'NONE', #18526 ) ;
#18288 = CARTESIAN_POINT ( 'NONE',  ( 9.500000000000209610, -3.086737114211962396, 11.10674201446023446 ) ) ;
#18289 = CARTESIAN_POINT ( 'NONE',  ( -5.871322893123450015, -8.081182679344781405, 8.506742014460233037 ) ) ;
#18290 = ORIENTED_EDGE ( 'NONE', *, *, #2608, .F. ) ;
#18291 = ORIENTED_EDGE ( 'NONE', *, *, #12676, .T. ) ;
#18292 = DIRECTION ( 'NONE',  ( 5.881959408733300741E-17, 6.514579901860026101E-17, -1.000000000000000000 ) ) ;
#18293 = DIRECTION ( 'NONE',  ( -1.000000000000000000, 0.000000000000000000, 0.000000000000000000 ) ) ;
#18294 = DIRECTION ( 'NONE',  ( 0.000000000000000000, -1.000000000000000000, 0.000000000000000000 ) ) ;
#18295 = CARTESIAN_POINT ( 'NONE',  ( -42.00000000000000000, 0.000000000000000000, 0.000000000000000000 ) ) ;
#18296 = DIRECTION ( 'NONE',  ( 0.000000000000000000, -1.000000000000000000, 0.000000000000000000 ) ) ;
#18297 = DIRECTION ( 'NONE',  ( -0.000000000000000000, -0.000000000000000000, 1.000000000000000000 ) ) ;
#18298 = EDGE_CURVE ( 'NONE', #25, #12017, #9353, .T. ) ;
#18299 = ORIENTED_EDGE ( 'NONE', *, *, #21444, .F. ) ;
#18300 = TOROIDAL_SURFACE ( 'NONE', #22577, 10.02592346138681023, 0.2999999999999999334 ) ;
#18301 = VERTEX_POINT ( 'NONE', #16783 ) ;
#18302 = SURFACE_STYLE_USAGE ( .BOTH. , #5121 ) ;
#18303 = DIRECTION ( 'NONE',  ( -1.000000000000000000, 0.000000000000000000, 0.000000000000000000 ) ) ;
#18304 = CARTESIAN_POINT ( 'NONE',  ( -9.440377765553483513, 1.232704728397706839, -3.501569427774944732 ) ) ;
#18305 = CARTESIAN_POINT ( 'NONE',  ( -7.685661446561619314, -5.583959896779019161, -11.25958914175814307 ) ) ;
#18306 = EDGE_CURVE ( 'NONE', #20942, #10396, #15600, .T. ) ;
#18307 = DIRECTION ( 'NONE',  ( -1.000000000000000000, 0.000000000000000000, 0.000000000000000000 ) ) ;
#18308 = CARTESIAN_POINT ( 'NONE',  ( -5.365059087798939252, -7.384370330707086261, -7.933165578109187877 ) ) ;
#18309 = EDGE_CURVE ( 'NONE', #23706, #11173, #3156, .T. ) ;
#18310 = AXIS2_PLACEMENT_3D ( 'NONE', #21470, #15477, #11804 ) ;
#18311 = FACE_OUTER_BOUND ( 'NONE', #950, .T. ) ;
#18312 = VERTEX_POINT ( 'NONE', #18750 ) ;
#18313 = DIRECTION ( 'NONE',  ( 0.000000000000000000, -1.000000000000000000, 0.000000000000000000 ) ) ;
#18314 = ORIENTED_EDGE ( 'NONE', *, *, #10621, .T. ) ;
#18315 = CIRCLE ( 'NONE', #5439, 1.024999999999999911 ) ;
#18316 = DIRECTION ( 'NONE',  ( -0.000000000000000000, -0.000000000000000000, -1.000000000000000000 ) ) ;
#18317 = EDGE_LOOP ( 'NONE', ( #16883, #20887, #9159, #5326 ) ) ;
#18318 = DIRECTION ( 'NONE',  ( 0.000000000000000000, -1.000000000000000000, 0.000000000000000000 ) ) ;
#18319 = CARTESIAN_POINT ( 'NONE',  ( -2.024999999999999911, 45.00000000000000000, -27.00000000000000000 ) ) ;
#18320 = LINE ( 'NONE', #3546, #20479 ) ;
#18321 = ORIENTED_EDGE ( 'NONE', *, *, #23322, .F. ) ;
#18322 = CARTESIAN_POINT ( 'NONE',  ( 0.000000000000000000, 0.000000000000000000, 3.499999999999999556 ) ) ;
#18323 = FACE_OUTER_BOUND ( 'NONE', #2164, .T. ) ;
#18324 = CARTESIAN_POINT ( 'NONE',  ( 6.809999908187194197E-13, -9.988891130263535700, -9.559589141758145558 ) ) ;
#18325 = EDGE_LOOP ( 'NONE', ( #11237, #18207 ) ) ;
#18326 = DIRECTION ( 'NONE',  ( -0.000000000000000000, -0.000000000000000000, 1.000000000000000000 ) ) ;
#18327 = VECTOR ( 'NONE', #6609, 1000.000000000000000 ) ;
#18328 = ADVANCED_FACE ( 'NONE', ( #20839 ), #23442, .T. ) ;
#18329 = DIRECTION ( 'NONE',  ( -1.000000000000000000, -1.224606353822377258E-16, -0.000000000000000000 ) ) ;
#18330 = MANIFOLD_SOLID_BREP ( 'Chamfer1', #14355 ) ;
#18331 = ORIENTED_EDGE ( 'NONE', *, *, #2150, .F. ) ;
#18332 = ADVANCED_FACE ( 'NONE', ( #7863 ), #16016, .F. ) ;
#18333 = CARTESIAN_POINT ( 'NONE',  ( -42.00000000000000000, 25.22443390181683043, -3.000000000000000000 ) ) ;
#18334 = DIRECTION ( 'NONE',  ( 0.000000000000000000, 0.000000000000000000, 1.000000000000000000 ) ) ;
#18335 = DIRECTION ( 'NONE',  ( -1.000000000000000000, -1.224606353822377258E-16, -0.000000000000000000 ) ) ;
#18336 = ORIENTED_EDGE ( 'NONE', *, *, #7056, .T. ) ;
#18337 = LINE ( 'NONE', #5055, #9489 ) ;
#18338 = CARTESIAN_POINT ( 'NONE',  ( 33.99999999999998579, -1.387778780781445676E-14, 9.500000000000000000 ) ) ;
#18339 = DIRECTION ( 'NONE',  ( 0.000000000000000000, 0.4999999999999989453, -0.8660254037844392627 ) ) ;
#18340 = CARTESIAN_POINT ( 'NONE',  ( 0.000000000000000000, 45.00000000000000000, -8.673617379884035472E-16 ) ) ;
#18341 = CIRCLE ( 'NONE', #13652, 17.87500000001787726 ) ;
#18342 = VERTEX_POINT ( 'NONE', #22911 ) ;
#18343 = ORIENTED_EDGE ( 'NONE', *, *, #6530, .T. ) ;
#18344 = VERTEX_POINT ( 'NONE', #15184 ) ;
#18345 = DIRECTION ( 'NONE',  ( 0.000000000000000000, -1.000000000000000000, 0.000000000000000000 ) ) ;
#18346 = EDGE_CURVE ( 'NONE', #22249, #18312, #20593, .T. ) ;
#18347 = FACE_OUTER_BOUND ( 'NONE', #2663, .T. ) ;
#18348 = VERTEX_POINT ( 'NONE', #21062 ) ;
#18349 = EDGE_CURVE ( 'NONE', #13485, #1630, #17830, .T. ) ;
#18350 = CYLINDRICAL_SURFACE ( 'NONE', #14573, 9.500000000000000000 ) ;
#18351 = ORIENTED_EDGE ( 'NONE', *, *, #3676, .F. ) ;
#18352 = CARTESIAN_POINT ( 'NONE',  ( 3.890962118697714531E-15, 15.50000000000000000, 14.70000000000000284 ) ) ;
#18353 = CARTESIAN_POINT ( 'NONE',  ( 3.890962118697714531E-15, 15.50000000000000000, 7.700000000000001954 ) ) ;
#18354 = AXIS2_PLACEMENT_3D ( 'NONE', #23021, #3021, #17409 ) ;
#18355 = CYLINDRICAL_SURFACE ( 'NONE', #5060, 8.000000000000003553 ) ;
#18356 = CARTESIAN_POINT ( 'NONE',  ( -31.74999999999995737, 0.000000000000000000, 5.000000000000000888 ) ) ;
#18357 = DIRECTION ( 'NONE',  ( 1.000000000000000000, 0.000000000000000000, 0.000000000000000000 ) ) ;
#18358 = CIRCLE ( 'NONE', #19143, 11.00000000000000000 ) ;
#18359 = DIRECTION ( 'NONE',  ( -1.360567432138674546E-16, 1.000000000000000000, 0.000000000000000000 ) ) ;
#18360 = CARTESIAN_POINT ( 'NONE',  ( -41.50000000000000000, 28.80990663662250739, 11.00000000000000000 ) ) ;
#18361 = DIRECTION ( 'NONE',  ( -0.000000000000000000, -0.000000000000000000, -1.000000000000000000 ) ) ;
#18362 = DIRECTION ( 'NONE',  ( -0.000000000000000000, -0.000000000000000000, -1.000000000000000000 ) ) ;
#18363 = CARTESIAN_POINT ( 'NONE',  ( 8.680847955711007202, 5.912916378492122225E-13, 8.633165578109188942 ) ) ;
#18364 = MANIFOLD_SOLID_BREP ( '\X2\00d8\X0\4.0mm Dowel Hole1', #3847 ) ;
#18365 = ORIENTED_EDGE ( 'NONE', *, *, #19323, .T. ) ;
#18366 = APPLICATION_PROTOCOL_DEFINITION ( 'draft international standard', 'automotive_design', 1998, #23974 ) ;
#18367 = CARTESIAN_POINT ( 'NONE',  ( 9.999999999999998224, 1.224646799147353059E-15, 15.50000000000000000 ) ) ;
#18368 = VECTOR ( 'NONE', #17833, 1000.000000000000000 ) ;
#18369 = ORIENTED_EDGE ( 'NONE', *, *, #18944, .F. ) ;
#18370 = ORIENTED_EDGE ( 'NONE', *, *, #18092, .F. ) ;
#18371 =( REPRESENTATION_RELATIONSHIP ('NONE','NONE', #5350, #23741 ) REPRESENTATION_RELATIONSHIP_WITH_TRANSFORMATION ( #19318 )SHAPE_REPRESENTATION_RELATIONSHIP( ) );
#18372 = VECTOR ( 'NONE', #4344, 1000.000000000000000 ) ;
#18373 = DIRECTION ( 'NONE',  ( 0.9945797436152712390, -0.1039766011667123125, -2.300427773307206454E-15 ) ) ;
#18374 = CARTESIAN_POINT ( 'NONE',  ( -5.871322893124554021, 8.081182679343978492, -6.759589141758143072 ) ) ;
#18375 = ADVANCED_FACE ( 'NONE', ( #11903 ), #19007, .T. ) ;
#18376 = CIRCLE ( 'NONE', #5533, 50.00000000000000000 ) ;
#18377 = DIRECTION ( 'NONE',  ( -0.000000000000000000, -0.000000000000000000, 1.000000000000000000 ) ) ;
#18378 = CARTESIAN_POINT ( 'NONE',  ( 6.250000000000000000, -10.82531754730548279, 2.500000000000000000 ) ) ;
#18379 = EDGE_CURVE ( 'NONE', #10172, #6915, #21438, .T. ) ;
#18380 = EDGE_CURVE ( 'NONE', #13723, #23530, #1218, .T. ) ;
#18381 = CARTESIAN_POINT ( 'NONE',  ( -8.000000000000000000, 9.797174393178825657E-16, -12.50000000000000000 ) ) ;
#18382 = ORIENTED_EDGE ( 'NONE', *, *, #5753, .F. ) ;
#18383 = LINE ( 'NONE', #5342, #18028 ) ;
#18384 = ORIENTED_EDGE ( 'NONE', *, *, #22382, .T. ) ;
#18385 = CARTESIAN_POINT ( 'NONE',  ( 0.000000000000000000, 2.967071445750145031, -17.62702788437270840 ) ) ;
#18386 = DIRECTION ( 'NONE',  ( 0.000000000000000000, -1.000000000000000000, 0.000000000000000000 ) ) ;
#18387 = DIRECTION ( 'NONE',  ( 0.000000000000000000, 0.000000000000000000, 1.000000000000000000 ) ) ;
#18388 = CARTESIAN_POINT ( 'NONE',  ( 0.000000000000000000, 0.000000000000000000, 51.99999999999998579 ) ) ;
#18389 = CONICAL_SURFACE ( 'NONE', #18763, 5.000000000000007994, 0.9599310885968855844 ) ;
#18390 = CIRCLE ( 'NONE', #14533, 1.500000000000000222 ) ;
#18391 = CYLINDRICAL_SURFACE ( 'NONE', #9109, 18.50000000000000000 ) ;
#18392 = DIRECTION ( 'NONE',  ( 0.000000000000000000, 0.000000000000000000, 1.000000000000000000 ) ) ;
#18393 = FILL_AREA_STYLE ('',( #14608 ) ) ;
#18394 = VERTEX_POINT ( 'NONE', #8228 ) ;
#18395 = ORIENTED_EDGE ( 'NONE', *, *, #9142, .F. ) ;
#18396 = CARTESIAN_POINT ( 'NONE',  ( -9.500000000000000000, -6.482511860946779655E-13, 8.206742014460234103 ) ) ;
#18397 = CARTESIAN_POINT ( 'NONE',  ( 5.871322893124553133, -8.081182679343980269, 4.906742014460232504 ) ) ;
#18398 = FACE_OUTER_BOUND ( 'NONE', #6995, .T. ) ;
#18399 = EDGE_LOOP ( 'NONE', ( #15901, #19689 ) ) ;
#18400 = EDGE_LOOP ( 'NONE', ( #2346, #3529 ) ) ;
#18401 = EDGE_CURVE ( 'NONE', #3687, #15969, #3928, .T. ) ;
#18402 = CARTESIAN_POINT ( 'NONE',  ( 66.14750088563508257, 7.420530141404717394E-15, 0.000000000000000000 ) ) ;
#18403 = CARTESIAN_POINT ( 'NONE',  ( -28.99999999999999645, -29.50000000000000000, -3.000000000000000000 ) ) ;
#18404 = ADVANCED_FACE ( 'NONE', ( #17517 ), #10144, .T. ) ;
#18405 = AXIS2_PLACEMENT_3D ( 'NONE', #16551, #3620, #7282 ) ;
#18406 = CARTESIAN_POINT ( 'NONE',  ( 0.000000000000000000, -8.772759796005177080, -7.720943453482119523 ) ) ;
#18407 = CIRCLE ( 'NONE', #2414, 9.000000000000000000 ) ;
#18408 = FACE_OUTER_BOUND ( 'NONE', #10849, .T. ) ;
#18409 = EDGE_CURVE ( 'NONE', #16640, #23003, #10440, .T. ) ;
#18410 = AXIS2_PLACEMENT_3D ( 'NONE', #16472, #5390, #10852 ) ;
#18411 = AXIS2_PLACEMENT_3D ( 'NONE', #11428, #22932, #11669 ) ;
#18412 = ADVANCED_FACE ( 'NONE', ( #1075 ), #20684, .T. ) ;
#18413 = AXIS2_PLACEMENT_3D ( 'NONE', #20357, #8892, #9347 ) ;
#18414 = AXIS2_PLACEMENT_3D ( 'NONE', #20919, #19337, #6523 ) ;
#18415 = ORIENTED_EDGE ( 'NONE', *, *, #5870, .F. ) ;
#18416 = AXIS2_PLACEMENT_3D ( 'NONE', #10761, #1272, #3338 ) ;
#18417 = CARTESIAN_POINT ( 'NONE',  ( -41.73082370883257397, -27.62204025492845361, -3.000000000000000000 ) ) ;
#18418 = DIRECTION ( 'NONE',  ( 0.000000000000000000, 0.000000000000000000, 1.000000000000000000 ) ) ;
#18419 = DIRECTION ( 'NONE',  ( 1.000000000000000000, 0.000000000000000000, 0.000000000000000000 ) ) ;
#18420 = CARTESIAN_POINT ( 'NONE',  ( 77.48886275072855767, -1.078520768856852078E-29, 5.000000000000007994 ) ) ;
#18421 = DIRECTION ( 'NONE',  ( 0.000000000000000000, 0.000000000000000000, 1.000000000000000000 ) ) ;
#18422 = CARTESIAN_POINT ( 'NONE',  ( -6.233975306307046963E-13, 9.127583699786111282, -9.133165578109188942 ) ) ;
#18423 = LINE ( 'NONE', #19903, #16573 ) ;
#18424 = ORIENTED_EDGE ( 'NONE', *, *, #8706, .T. ) ;
#18425 = DIRECTION ( 'NONE',  ( 1.000000000000000000, 0.000000000000000000, 0.000000000000000000 ) ) ;
#18426 = ORIENTED_EDGE ( 'NONE', *, *, #3960, .T. ) ;
#18427 = VECTOR ( 'NONE', #8616, 1000.000000000000000 ) ;
#18428 = AXIS2_PLACEMENT_3D ( 'NONE', #3533, #18070, #7311 ) ;
#18429 = AXIS2_PLACEMENT_3D ( 'NONE', #20659, #18830, #20049 ) ;
#18430 = CIRCLE ( 'NONE', #21162, 4.172000000000008590 ) ;
#18431 = ORIENTED_EDGE ( 'NONE', *, *, #20721, .F. ) ;
#18432 = CARTESIAN_POINT ( 'NONE',  ( 41.99999999999997868, -25.22443390181679845, -0.6213203435596419411 ) ) ;
#18433 = AXIS2_PLACEMENT_3D ( 'NONE', #15010, #22365, #5644 ) ;
#18434 = DIRECTION ( 'NONE',  ( -1.000000000000000000, -1.224606353822377258E-16, -0.000000000000000000 ) ) ;
#18435 = EDGE_CURVE ( 'NONE', #2518, #5912, #4727, .T. ) ;
#18436 = CARTESIAN_POINT ( 'NONE',  ( -40.99749999999999517, 0.000000000000000000, 0.000000000000000000 ) ) ;
#18437 = AXIS2_PLACEMENT_3D ( 'NONE', #6730, #260, #12919 ) ;
#18438 = LINE ( 'NONE', #1729, #2560 ) ;
#18439 = VECTOR ( 'NONE', #205, 1000.000000000000000 ) ;
#18440 = DIRECTION ( 'NONE',  ( -1.000000000000000000, 0.000000000000000000, 0.000000000000000000 ) ) ;
#18441 = ADVANCED_FACE ( 'NONE', ( #4497 ), #15683, .F. ) ;
#18442 = EDGE_CURVE ( 'NONE', #19097, #13956, #12133, .T. ) ;
#18443 = CARTESIAN_POINT ( 'NONE',  ( 9.500000000000000000, 6.470877716354879437E-13, -6.059589141758143782 ) ) ;
#18444 = VERTEX_POINT ( 'NONE', #23156 ) ;
#18445 = ORIENTED_EDGE ( 'NONE', *, *, #13976, .F. ) ;
#18446 = CARTESIAN_POINT ( 'NONE',  ( 23.00000000000000000, -13.61176534793449200, 4.089617900950054619 ) ) ;
#18447 = DIRECTION ( 'NONE',  ( 1.000000000000000000, 0.000000000000000000, 0.000000000000000000 ) ) ;
#18448 = CIRCLE ( 'NONE', #7898, 1.000000000000000888 ) ;
#18449 = CIRCLE ( 'NONE', #524, 5.000000000000007994 ) ;
#18450 = CONICAL_SURFACE ( 'NONE', #4850, 4.172000000000008590, 0.9599310885968742602 ) ;
#18451 = CARTESIAN_POINT ( 'NONE',  ( 8.999999999999996447, 6.130305204967778181E-13, -12.50000000000000000 ) ) ;
#18452 = AXIS2_PLACEMENT_3D ( 'NONE', #1919, #2162, #13507 ) ;
#18453 = AXIS2_PLACEMENT_3D ( 'NONE', #17600, #909, #21407 ) ;
#18454 = ORIENTED_EDGE ( 'NONE', *, *, #16791, .T. ) ;
#18455 = AXIS2_PLACEMENT_3D ( 'NONE', #4406, #4282, #11815 ) ;
#18456 = LINE ( 'NONE', #12826, #4005 ) ;
#18457 = DIRECTION ( 'NONE',  ( 0.000000000000000000, 0.000000000000000000, -1.000000000000000000 ) ) ;
#18458 = LINE ( 'NONE', #1744, #16447 ) ;
#18459 = ORIENTED_EDGE ( 'NONE', *, *, #4163, .F. ) ;
#18460 = DIRECTION ( 'NONE',  ( -1.000000000000000000, 0.000000000000000000, 0.000000000000000000 ) ) ;
#18461 = CARTESIAN_POINT ( 'NONE',  ( 40.29291594121673370, -26.62062637246459218, 12.00000000000000000 ) ) ;
#18462 = CARTESIAN_POINT ( 'NONE',  ( -5.871322893124554021, 8.081182679343978492, -3.906742014460231616 ) ) ;
#18463 = CARTESIAN_POINT ( 'NONE',  ( 6.222797240145152671E-13, -9.127583699786111282, 6.133165578109188942 ) ) ;
#18464 = ORIENTED_EDGE ( 'NONE', *, *, #17926, .F. ) ;
#18465 = ORIENTED_EDGE ( 'NONE', *, *, #12029, .F. ) ;
#18466 = VERTEX_POINT ( 'NONE', #3125 ) ;
#18467 = AXIS2_PLACEMENT_3D ( 'NONE', #8349, #23266, #17758 ) ;
#18469 = VERTEX_POINT ( 'NONE', #21193 ) ;
#18468 = CIRCLE ( 'NONE', #18101, 1.000000000000000000 ) ;
#18470 = PLANE ( 'NONE',  #4109 ) ;
#18471 = ADVANCED_FACE ( 'NONE', ( #8369 ), #8591, .F. ) ;
#18472 = AXIS2_PLACEMENT_3D ( 'NONE', #19975, #1453, #16301 ) ;
#18473 = EDGE_CURVE ( 'NONE', #4017, #3844, #22636, .T. ) ;
#18474 = DIRECTION ( 'NONE',  ( -1.000000000000000000, -1.224606353822377258E-16, -0.000000000000000000 ) ) ;
#18475 = ORIENTED_EDGE ( 'NONE', *, *, #15339, .F. ) ;
#18476 = VECTOR ( 'NONE', #11430, 1000.000000000000000 ) ;
#18477 = FACE_OUTER_BOUND ( 'NONE', #18488, .T. ) ;
#18478 = ORIENTED_EDGE ( 'NONE', *, *, #18153, .T. ) ;
#18479 = CARTESIAN_POINT ( 'NONE',  ( 40.99749999999998096, 6.781874047275040887E-15, 9.499999999999989342 ) ) ;
#18480 = LINE ( 'NONE', #7129, #19948 ) ;
#18481 = FACE_BOUND ( 'NONE', #15533, .T. ) ;
#18482 = CIRCLE ( 'NONE', #1734, 5.000000000000007994 ) ;
#18483 = FACE_BOUND ( 'NONE', #14323, .T. ) ;
#18484 = DIRECTION ( 'NONE',  ( -1.000000000000000000, -1.224606353822377258E-16, -0.000000000000000000 ) ) ;
#18485 = CYLINDRICAL_SURFACE ( 'NONE', #3261, 4.499999999999997335 ) ;
#18486 = EDGE_CURVE ( 'NONE', #8001, #1469, #14102, .T. ) ;
#18487 = FACE_OUTER_BOUND ( 'NONE', #2531, .T. ) ;
#18488 = EDGE_LOOP ( 'NONE', ( #1168, #2633, #17121, #5032, #6011 ) ) ;
#18489 = AXIS2_PLACEMENT_3D ( 'NONE', #10750, #22130, #23818 ) ;
#18490 = ORIENTED_EDGE ( 'NONE', *, *, #7305, .F. ) ;
#18491 = CARTESIAN_POINT ( 'NONE',  ( 2.682529543900284974, -8.255977015246234174, 12.23316557810919036 ) ) ;
#18492 = ORIENTED_EDGE ( 'NONE', *, *, #15051, .F. ) ;
#18493 = AXIS2_PLACEMENT_3D ( 'NONE', #10813, #12884, #24010 ) ;
#18494 = EDGE_CURVE ( 'NONE', #6052, #19513, #4735, .T. ) ;
#18495 = APPLICATION_PROTOCOL_DEFINITION ( 'draft international standard', 'automotive_design', 1998, #9439 ) ;
#18496 = EDGE_CURVE ( 'NONE', #4711, #17959, #12271, .T. ) ;
#18497 = DIRECTION ( 'NONE',  ( -1.000000000000000000, -0.000000000000000000, -0.000000000000000000 ) ) ;
#18498 = VERTEX_POINT ( 'NONE', #10063 ) ;
#18499 = VERTEX_POINT ( 'NONE', #19741 ) ;
#18500 = EDGE_CURVE ( 'NONE', #13857, #19153, #7808, .T. ) ;
#18501 = DIRECTION ( 'NONE',  ( -1.000000000000000000, 0.000000000000000000, 0.000000000000000000 ) ) ;
#18502 = CARTESIAN_POINT ( 'NONE',  ( 2.682529543900284974, -8.255977015246234174, -8.233165578109190363 ) ) ;
#18503 = CIRCLE ( 'NONE', #10309, 9.000000000000000000 ) ;
#18504 = VECTOR ( 'NONE', #6260, 1000.000000000000000 ) ;
#18505 = EDGE_LOOP ( 'NONE', ( #24071, #4007, #9384 ) ) ;
#18506 = CARTESIAN_POINT ( 'NONE',  ( 1.016919733032271456, 45.00000000000000000, 3.000000000000002665 ) ) ;
#18507 = DIRECTION ( 'NONE',  ( -0.000000000000000000, -0.000000000000000000, -1.000000000000000000 ) ) ;
#18508 = CARTESIAN_POINT ( 'NONE',  ( 31.49999999999999289, -51.00000000000000711, 12.50000000000000000 ) ) ;
#18509 = CARTESIAN_POINT ( 'NONE',  ( 10.00000000000000533, 15.50000000000000000, 7.699999999999998401 ) ) ;
#18510 = CIRCLE ( 'NONE', #9510, 11.22592346138681130 ) ;
#18511 = CARTESIAN_POINT ( 'NONE',  ( 40.99749999999998096, 5.618459588085056979E-15, 0.000000000000000000 ) ) ;
#18512 = ORIENTED_EDGE ( 'NONE', *, *, #4031, .F. ) ;
#18513 = CARTESIAN_POINT ( 'NONE',  ( 0.000000000000000000, -15.03999999999999737, 2.200000000000000178 ) ) ;
#18514 = VERTEX_POINT ( 'NONE', #818 ) ;
#18515 = VERTEX_POINT ( 'NONE', #14337 ) ;
#18516 = CARTESIAN_POINT ( 'NONE',  ( 23.90000000000000568, 29.50000000000000355, 0.000000000000000000 ) ) ;
#18517 = CARTESIAN_POINT ( 'NONE',  ( 23.00000000000000000, -6.393861490227802591, -9.782270569456514409 ) ) ;
#18518 = DIRECTION ( 'NONE',  ( -0.000000000000000000, -0.000000000000000000, -1.000000000000000000 ) ) ;
#18519 = CARTESIAN_POINT ( 'NONE',  ( 80.69295543108962931, 7.420530141404717394E-15, 0.000000000000000000 ) ) ;
#18520 = VECTOR ( 'NONE', #15694, 1000.000000000000000 ) ;
#18521 = CIRCLE ( 'NONE', #7225, 11.68650000001168721 ) ;
#18522 = DIRECTION ( 'NONE',  ( -0.8571673007021116675, 0.000000000000000000, -0.5150380749100552658 ) ) ;
#18523 = DIRECTION ( 'NONE',  ( -1.000000000000000000, -1.224606353822377258E-16, -0.000000000000000000 ) ) ;
#18525 = ADVANCED_FACE ( 'NONE', ( #7019 ), #7059, .F. ) ;
#18524 = CARTESIAN_POINT ( 'NONE',  ( 5.871322893124553133, -8.081182679343980269, -10.90674201446023339 ) ) ;
#18526 = CARTESIAN_POINT ( 'NONE',  ( 1.999999999999997113, 45.00000000000000000, -2.974999999999996092 ) ) ;
#18527 = VERTEX_POINT ( 'NONE', #8730 ) ;
#18528 = ORIENTED_EDGE ( 'NONE', *, *, #3289, .T. ) ;
#18529 = CARTESIAN_POINT ( 'NONE',  ( 7.685661446562381371, -5.583959896777971110, 7.006742014460233037 ) ) ;
#18530 = EDGE_CURVE ( 'NONE', #18883, #21492, #10162, .T. ) ;
#18531 = ORIENTED_EDGE ( 'NONE', *, *, #6931, .F. ) ;
#18532 = ORIENTED_EDGE ( 'NONE', *, *, #155, .T. ) ;
#18533 = AXIS2_PLACEMENT_3D ( 'NONE', #658, #11601, #8066 ) ;
#18534 = DIRECTION ( 'NONE',  ( -0.000000000000000000, 0.000000000000000000, 1.000000000000000000 ) ) ;
#18535 = AXIS2_PLACEMENT_3D ( 'NONE', #20384, #10739, #10853 ) ;
#18536 = ORIENTED_EDGE ( 'NONE', *, *, #4369, .T. ) ;
#18537 = DIRECTION ( 'NONE',  ( -1.000000000000000000, -1.224606353822377258E-16, -0.000000000000000000 ) ) ;
#18538 = DIRECTION ( 'NONE',  ( -1.000000000000000000, -1.224606353822377258E-16, -0.000000000000000000 ) ) ;
#18539 = VECTOR ( 'NONE', #6554, 1000.000000000000000 ) ;
#18540 = AXIS2_PLACEMENT_3D ( 'NONE', #19304, #1005, #6611 ) ;
#18541 = DIRECTION ( 'NONE',  ( -0.000000000000000000, -0.000000000000000000, -1.000000000000000000 ) ) ;
#18542 =( NAMED_UNIT ( * ) SI_UNIT ( $, .STERADIAN. ) SOLID_ANGLE_UNIT ( ) );
#18543 = CARTESIAN_POINT ( 'NONE',  ( -28.99999999999999645, -29.50000000000000000, 12.50000000000000000 ) ) ;
#18544 = ORIENTED_EDGE ( 'NONE', *, *, #4913, .F. ) ;
#18545 = AXIS2_PLACEMENT_3D ( 'NONE', #2967, #6868, #6743 ) ;
#18546 = DIRECTION ( 'NONE',  ( 0.000000000000000000, 0.000000000000000000, 1.000000000000000000 ) ) ;
#18547 = CARTESIAN_POINT ( 'NONE',  ( 40.00000000000000000, 29.49999999999999645, 12.00000000000000000 ) ) ;
#18548 = DIRECTION ( 'NONE',  ( -0.000000000000000000, -0.000000000000000000, -1.000000000000000000 ) ) ;
#18549 = CARTESIAN_POINT ( 'NONE',  ( 9.330908268522616567, -1.784418920661929642, -11.99999999999998934 ) ) ;
#18550 =( GEOMETRIC_REPRESENTATION_CONTEXT ( 3 ) GLOBAL_UNCERTAINTY_ASSIGNED_CONTEXT ( ( #6684 ) ) GLOBAL_UNIT_ASSIGNED_CONTEXT ( ( #10220, #12423, #7178 ) ) REPRESENTATION_CONTEXT ( 'NONE', 'WORKASPACE' ) );
#18551 = CIRCLE ( 'NONE', #9568, 6.050000000006050982 ) ;
#18552 = LINE ( 'NONE', #14390, #7388 ) ;
#18553 = CARTESIAN_POINT ( 'NONE',  ( 8.680847955711199049, -2.820578480813074496, -10.53316557810918752 ) ) ;
#18554 = VECTOR ( 'NONE', #23324, 1000.000000000000000 ) ;
#18555 = CARTESIAN_POINT ( 'NONE',  ( -29.00000000000000000, 29.49999999999999645, 12.00000000000000000 ) ) ;
#18556 = EDGE_CURVE ( 'NONE', #13716, #19319, #14445, .T. ) ;
#18557 = AXIS2_PLACEMENT_3D ( 'NONE', #10638, #12471, #22138 ) ;
#18558 = CIRCLE ( 'NONE', #7258, 4.172000000000008590 ) ;
#18559 = ORIENTED_EDGE ( 'NONE', *, *, #19102, .T. ) ;
#18560 = PLANE ( 'NONE',  #21224 ) ;
#18561 = EDGE_LOOP ( 'NONE', ( #23200, #14112, #4947, #14464 ) ) ;
#18562 = LINE ( 'NONE', #13045, #23515 ) ;
#18563 = ADVANCED_FACE ( 'NONE', ( #1307 ), #21386, .F. ) ;
#18564 = DIRECTION ( 'NONE',  ( -1.000000000000000000, -1.224606353822377258E-16, -0.000000000000000000 ) ) ;
#18565 = ADVANCED_FACE ( 'NONE', ( #1519 ), #22657, .F. ) ;
#18566 = ORIENTED_EDGE ( 'NONE', *, *, #3709, .F. ) ;
#18567 = CARTESIAN_POINT ( 'NONE',  ( 29.00000000000000000, -29.50000000000000355, 11.50000000000000000 ) ) ;
#18568 = CARTESIAN_POINT ( 'NONE',  ( 0.000000000000000000, 0.000000000000000000, 13.72592346138681130 ) ) ;
#18569 = CARTESIAN_POINT ( 'NONE',  ( -23.85000000000000142, -15.03999999999999737, 0.000000000000000000 ) ) ;
#18570 = CIRCLE ( 'NONE', #22472, 6.050000000006050094 ) ;
#18571 = PRODUCT_DEFINITION_FORMATION_WITH_SPECIFIED_SOURCE ( 'ANY', '', #5703, .NOT_KNOWN. ) ;
#18572 = VECTOR ( 'NONE', #6651, 1000.000000000000000 ) ;
#18573 = AXIS2_PLACEMENT_3D ( 'NONE', #7692, #15130, #648 ) ;
#18574 = CARTESIAN_POINT ( 'NONE',  ( 2.935661446561383503, 9.035036904804158553, -8.459589141758144137 ) ) ;
#18575 = EDGE_LOOP ( 'NONE', ( #18595, #21918, #12526, #13582 ) ) ;
#18576 = VERTEX_POINT ( 'NONE', #12472 ) ;
#18577 = FACE_OUTER_BOUND ( 'NONE', #6365, .T. ) ;
#18578 = ORIENTED_EDGE ( 'NONE', *, *, #3201, .T. ) ;
#18579 = EDGE_CURVE ( 'NONE', #10046, #5101, #8826, .T. ) ;
#18580 = ORIENTED_EDGE ( 'NONE', *, *, #21395, .T. ) ;
#18581 = AXIS2_PLACEMENT_3D ( 'NONE', #7447, #4192, #18948 ) ;
#18582 = FACE_OUTER_BOUND ( 'NONE', #7678, .T. ) ;
#18583 = CARTESIAN_POINT ( 'NONE',  ( -28.99999999999999645, 29.50000000000000000, -3.000000000000000000 ) ) ;
#18584 = EDGE_CURVE ( 'NONE', #23464, #18617, #16148, .T. ) ;
#18585 = CARTESIAN_POINT ( 'NONE',  ( -34.00000000000000000, -3.851859888774471706E-31, 9.500000000000000000 ) ) ;
#18586 = ORIENTED_EDGE ( 'NONE', *, *, #5840, .F. ) ;
#18587 = CARTESIAN_POINT ( 'NONE',  ( 77.48886275072855767, 7.562528597612068045E-15, 0.000000000000000000 ) ) ;
#18588 = DIRECTION ( 'NONE',  ( 0.000000000000000000, -1.000000000000000000, 0.000000000000000000 ) ) ;
#18589 = ADVANCED_FACE ( 'NONE', ( #1274 ), #10764, .T. ) ;
#18590 = CARTESIAN_POINT ( 'NONE',  ( 6.809999908187194197E-13, -9.988891130263535700, -8.706742014460230550 ) ) ;
#18591 = DIRECTION ( 'NONE',  ( 0.000000000000000000, 0.000000000000000000, 1.000000000000000000 ) ) ;
#18592 = EDGE_CURVE ( 'NONE', #4737, #3391, #10553, .T. ) ;
#18593 = CYLINDRICAL_SURFACE ( 'NONE', #18581, 9.500000000000000000 ) ;
#18594 = CARTESIAN_POINT ( 'NONE',  ( -8.680847955710813579, -2.820578480814258437, 3.733165578109188587 ) ) ;
#18595 = ORIENTED_EDGE ( 'NONE', *, *, #2291, .T. ) ;
#18596 = ORIENTED_EDGE ( 'NONE', *, *, #21726, .T. ) ;
#18597 = EDGE_LOOP ( 'NONE', ( #23661, #11878 ) ) ;
#18598 = CARTESIAN_POINT ( 'NONE',  ( 73.12522638709218370, 7.562528597612068045E-15, 0.000000000000000000 ) ) ;
#18599 = DIRECTION ( 'NONE',  ( 0.000000000000000000, 0.000000000000000000, 1.000000000000000000 ) ) ;
#18600 = ORIENTED_EDGE ( 'NONE', *, *, #22723, .T. ) ;
#18601 = DIRECTION ( 'NONE',  ( -0.000000000000000000, -1.000000000000000000, -0.000000000000000000 ) ) ;
#18602 = VERTEX_POINT ( 'NONE', #3341 ) ;
#18603 =( BOUNDED_CURVE ( )  B_SPLINE_CURVE ( 2, ( #20007, #14029, #3287, #1352, #18186, #21475, #6476, #1479, #2802, #13917, #21360, #8411, #15862 ),
 .UNSPECIFIED., .F., .T. ) 
 B_SPLINE_CURVE_WITH_KNOTS ( ( 3, 2, 2, 2, 2, 2, 3 ),
 ( 0.8558632199373861216, 0.8599999999999999867, 0.8800000000000000044, 0.9000000000000000222, 0.9200000000000000400, 0.9399999999999999467, 0.9500000000000000666 ),
 .UNSPECIFIED. ) 
 CURVE ( )  GEOMETRIC_REPRESENTATION_ITEM ( )  RATIONAL_B_SPLINE_CURVE ( ( 0.9839409940142059829, 0.9898765786207461836, 1.000000000000000000, 0.9510565162951535312, 1.000000000000000000, 0.9510565162951535312, 1.000000000000000000, 0.9510565162951535312, 1.000000000000000000, 0.9510565162951535312, 1.000000000000000000, 0.9755282581475764880, 0.9755282581475768211 ) ) 
 REPRESENTATION_ITEM ( '' )  );
#18604 = EDGE_CURVE ( 'NONE', #13932, #12301, #14311, .T. ) ;
#18605 = FACE_OUTER_BOUND ( 'NONE', #21446, .T. ) ;
#18606 = FACE_BOUND ( 'NONE', #18399, .T. ) ;
#18607 = DIRECTION ( 'NONE',  ( -0.000000000000000000, -0.000000000000000000, 1.000000000000000000 ) ) ;
#18608 = CARTESIAN_POINT ( 'NONE',  ( -41.00000000000000000, 0.000000000000000000, 11.00000000000000000 ) ) ;
#18609 = LINE ( 'NONE', #13471, #23535 ) ;
#18610 = DIRECTION ( 'NONE',  ( -1.000000000000000000, 0.000000000000000000, 0.000000000000000000 ) ) ;
#18611 = CARTESIAN_POINT ( 'NONE',  ( 23.00000000000000000, 10.59264252385243665, -4.936618945406485714 ) ) ;
#18612 = VERTEX_POINT ( 'NONE', #23830 ) ;
#18613 = ADVANCED_FACE ( 'NONE', ( #7109 ), #14549, .T. ) ;
#18614 = VERTEX_POINT ( 'NONE', #10873 ) ;
#18615 = ADVANCED_BREP_SHAPE_REPRESENTATION ( '', ( #2885, #8005 ), #651 ) ;
#18616 = CARTESIAN_POINT ( 'NONE',  ( -2.935661446562617183, 9.035036904803758873, 10.65958914175814343 ) ) ;
#18617 = VERTEX_POINT ( 'NONE', #16502 ) ;
#18618 = APPLICATION_PROTOCOL_DEFINITION ( 'draft international standard', 'automotive_design', 1998, #13382 ) ;
#18619 = EDGE_LOOP ( 'NONE', ( #4643, #10191, #7589, #19000 ) ) ;
#18620 = ORIENTED_EDGE ( 'NONE', *, *, #1559, .T. ) ;
#18621 = LINE ( 'NONE', #10903, #5646 ) ;
#18622 = CARTESIAN_POINT ( 'NONE',  ( -5.871322893123450015, -8.081182679344781405, -3.359589141758143160 ) ) ;
#18623 = DIRECTION ( 'NONE',  ( 0.000000000000000000, 0.000000000000000000, 1.000000000000000000 ) ) ;
#18624 = ORIENTED_EDGE ( 'NONE', *, *, #4829, .T. ) ;
#18625 = LINE ( 'NONE', #11260, #14930 ) ;
#18626 = DIRECTION ( 'NONE',  ( 0.000000000000000000, 0.7557495743542551603, 0.6548607339452887643 ) ) ;
#18627 = CARTESIAN_POINT ( 'NONE',  ( -28.99999999999999645, -29.50000000000001066, -27.00000000000000000 ) ) ;
#18628 = ORIENTED_EDGE ( 'NONE', *, *, #12398, .T. ) ;
#18629 = CARTESIAN_POINT ( 'NONE',  ( 73.42022815836234884, 7.420530141404717394E-15, 0.000000000000000000 ) ) ;
#18630 = ORIENTED_EDGE ( 'NONE', *, *, #20336, .T. ) ;
#18631 = ADVANCED_FACE ( 'NONE', ( #12363 ), #23959, .T. ) ;
#18632 = ORIENTED_EDGE ( 'NONE', *, *, #5039, .T. ) ;
#18633 = CYLINDRICAL_SURFACE ( 'NONE', #19963, 5.000000000000000888 ) ;
#18634 = DIRECTION ( 'NONE',  ( -0.000000000000000000, -0.000000000000000000, 1.000000000000000000 ) ) ;
#18635 = CARTESIAN_POINT ( 'NONE',  ( -39.99999999999999289, 29.50000000000000000, 27.00000000000000000 ) ) ;
#18636 = DIRECTION ( 'NONE',  ( -1.000000000000000000, 0.000000000000000000, 0.000000000000000000 ) ) ;
#18637 = EDGE_CURVE ( 'NONE', #1819, #4077, #5058, .T. ) ;
#18638 = FACE_OUTER_BOUND ( 'NONE', #16407, .T. ) ;
#18639 = CARTESIAN_POINT ( 'NONE',  ( 21.85000000000000497, 16.67999999999999972, 12.00000000000000000 ) ) ;
#18640 = EDGE_CURVE ( 'NONE', #16505, #15077, #16028, .T. ) ;
#18641 = AXIS2_PLACEMENT_3D ( 'NONE', #11349, #15035, #16864 ) ;
#18642 = CARTESIAN_POINT ( 'NONE',  ( -31.74999999999995737, 0.000000000000000000, 0.000000000000000000 ) ) ;
#18643 = ORIENTED_EDGE ( 'NONE', *, *, #5472, .F. ) ;
#18644 = VERTEX_POINT ( 'NONE', #2810 ) ;
#18645 = CARTESIAN_POINT ( 'NONE',  ( -7.685661446561619314, -5.583959896779019161, 10.40674201446023339 ) ) ;
#18646 = VERTEX_POINT ( 'NONE', #748 ) ;
#18647 = ORIENTED_EDGE ( 'NONE', *, *, #7255, .T. ) ;
#18648 = AXIS2_PLACEMENT_3D ( 'NONE', #22506, #13205, #22387 ) ;
#18649 =( NAMED_UNIT ( * ) PLANE_ANGLE_UNIT ( ) SI_UNIT ( $, .RADIAN. ) );
#18650 = TOROIDAL_SURFACE ( 'NONE', #17875, 2.500000000000001776, 1.000000000000000000 ) ;
#18651 = VERTEX_POINT ( 'NONE', #21244 ) ;
#18652 = PLANE ( 'NONE',  #2934 ) ;
#18653 = FACE_OUTER_BOUND ( 'NONE', #5860, .T. ) ;
#18654 = CYLINDRICAL_SURFACE ( 'NONE', #11794, 1.000000000000000888 ) ;
#18655 =( NAMED_UNIT ( * ) PLANE_ANGLE_UNIT ( ) SI_UNIT ( $, .RADIAN. ) );
#18656 = CARTESIAN_POINT ( 'NONE',  ( 3.373806935227752118E-18, 0.000000000000000000, 0.000000000000000000 ) ) ;
#18657 = EDGE_CURVE ( 'NONE', #18348, #578, #21878, .T. ) ;
#18658 = CARTESIAN_POINT ( 'NONE',  ( -5.871322893124554021, 8.081182679343978492, -10.75958914175814130 ) ) ;
#18659 = ORIENTED_EDGE ( 'NONE', *, *, #13476, .T. ) ;
#18660 = EDGE_CURVE ( 'NONE', #2307, #16483, #20321, .T. ) ;
#18661 = DIRECTION ( 'NONE',  ( -0.000000000000000000, -0.000000000000000000, -1.000000000000000000 ) ) ;
#18662 = DIRECTION ( 'NONE',  ( -4.613626265895763066E-16, -1.000000000000000000, 0.000000000000000000 ) ) ;
#18663 = CARTESIAN_POINT ( 'NONE',  ( -16.99687406587156602, 7.923972684219727114, -5.245599057861380032 ) ) ;
#18664 = DIRECTION ( 'NONE',  ( 0.000000000000000000, -1.000000000000000000, 0.000000000000000000 ) ) ;
#18665 = EDGE_CURVE ( 'NONE', #6367, #5961, #6719, .T. ) ;
#18666 = CARTESIAN_POINT ( 'NONE',  ( 9.499999999999998224, 0.000000000000000000, 15.50000000000000000 ) ) ;
#18667 = DIRECTION ( 'NONE',  ( -1.000000000000000000, -0.000000000000000000, -0.000000000000000000 ) ) ;
#18668 = EDGE_LOOP ( 'NONE', ( #2004, #312, #20418, #17658 ) ) ;
#18669 = CARTESIAN_POINT ( 'NONE',  ( 0.000000000000000000, 0.000000000000000000, 0.9999999999999731326 ) ) ;
#18670 = ORIENTED_EDGE ( 'NONE', *, *, #15051, .T. ) ;
#18671 = DIRECTION ( 'NONE',  ( -1.000000000000000000, 0.000000000000000000, 0.000000000000000000 ) ) ;
#18672 = ORIENTED_EDGE ( 'NONE', *, *, #19959, .F. ) ;
#18673 = PLANE ( 'NONE',  #8400 ) ;
#18674 = DIRECTION ( 'NONE',  ( 0.000000000000000000, 1.000000000000000000, -0.000000000000000000 ) ) ;
#18675 = DIRECTION ( 'NONE',  ( -1.000000000000000000, -1.224606353822377258E-16, -0.000000000000000000 ) ) ;
#18676 = LINE ( 'NONE', #22, #9939 ) ;
#18677 = DIRECTION ( 'NONE',  ( -1.000000000000000000, 0.000000000000000000, 0.000000000000000000 ) ) ;
#18678 = PLANE ( 'NONE',  #2476 ) ;
#18679 = CARTESIAN_POINT ( 'NONE',  ( 9.500000000000209610, -3.086737114211962396, -5.959589141758143249 ) ) ;
#18680 = ORIENTED_EDGE ( 'NONE', *, *, #13722, .T. ) ;
#18681 = DIRECTION ( 'NONE',  ( -0.000000000000000000, -0.000000000000000000, -1.000000000000000000 ) ) ;
#18682 = CARTESIAN_POINT ( 'NONE',  ( 5.871322893123448239, 8.081182679344781405, 11.50674201446023126 ) ) ;
#18683 = EDGE_CURVE ( 'NONE', #7839, #2862, #10939, .T. ) ;
#18684 = ADVANCED_FACE ( 'NONE', ( #6353 ), #23445, .T. ) ;
#18685 = ORIENTED_EDGE ( 'NONE', *, *, #3960, .F. ) ;
#18686 = CARTESIAN_POINT ( 'NONE',  ( -31.74999999999995737, 6.123233995736767268E-16, -5.000000000000000888 ) ) ;
#18687 = FACE_OUTER_BOUND ( 'NONE', #9379, .T. ) ;
#18688 = AXIS2_PLACEMENT_3D ( 'NONE', #811, #4722, #15673 ) ;
#18689 = ORIENTED_EDGE ( 'NONE', *, *, #5228, .F. ) ;
#18690 = DIRECTION ( 'NONE',  ( -1.000000000000000000, 0.000000000000000000, 0.000000000000000000 ) ) ;
#18691 = DIRECTION ( 'NONE',  ( -0.000000000000000000, -1.000000000000000000, -0.000000000000000000 ) ) ;
#18692 = CARTESIAN_POINT ( 'NONE',  ( 0.000000000000000000, 0.000000000000000000, 12.00000000000000000 ) ) ;
#18693 = VERTEX_POINT ( 'NONE', #4908 ) ;
#18694 = LINE ( 'NONE', #16844, #1954 ) ;
#18695 = DIRECTION ( 'NONE',  ( 0.000000000000000000, 0.9096319953545193293, -0.4154150130018841591 ) ) ;
#18696 = LINE ( 'NONE', #15384, #15052 ) ;
#18697 = CARTESIAN_POINT ( 'NONE',  ( -0.9830802669677229932, 45.00000000000000000, 0.02500000000000418554 ) ) ;
#18698 = VERTEX_POINT ( 'NONE', #4545 ) ;
#18699 = ORIENTED_EDGE ( 'NONE', *, *, #22303, .F. ) ;
#18700 = EDGE_LOOP ( 'NONE', ( #7320, #15651, #3406, #862 ) ) ;
#18701 = EDGE_CURVE ( 'NONE', #20733, #3712, #15873, .T. ) ;
#18702 = VECTOR ( 'NONE', #7313, 1000.000000000000000 ) ;
#18703 = ORIENTED_EDGE ( 'NONE', *, *, #11974, .T. ) ;
#18704 = LINE ( 'NONE', #14905, #4151 ) ;
#18705 = EDGE_CURVE ( 'NONE', #13107, #1819, #8622, .T. ) ;
#18706 = CARTESIAN_POINT ( 'NONE',  ( 23.00000000000000000, 11.37860023611340665, 13.78561139983856521 ) ) ;
#18707 = VERTEX_POINT ( 'NONE', #2695 ) ;
#18708 = EDGE_CURVE ( 'NONE', #22066, #8450, #16105, .T. ) ;
#18709 = ADVANCED_FACE ( 'NONE', ( #19418 ), #14152, .T. ) ;
#18710 = CYLINDRICAL_SURFACE ( 'NONE', #12343, 5.000000000000000888 ) ;
#18711 = ORIENTED_EDGE ( 'NONE', *, *, #22174, .F. ) ;
#18712 = DIRECTION ( 'NONE',  ( 0.000000000000000000, 0.7557495743542552713, 0.6548607339452886533 ) ) ;
#18713 = CYLINDRICAL_SURFACE ( 'NONE', #9046, 1.499999999999994449 ) ;
#18714 = FACE_OUTER_BOUND ( 'NONE', #12377, .T. ) ;
#18715 = CARTESIAN_POINT ( 'NONE',  ( 39.50000000000000000, 15.50000000000000533, 19.70000000000000284 ) ) ;
#18716 = COLOUR_RGB ( '',0.7921568627450980005, 0.8196078431372548767, 0.9333333333333333481 ) ;
#18717 = ORIENTED_EDGE ( 'NONE', *, *, #22699, .T. ) ;
#18718 = CARTESIAN_POINT ( 'NONE',  ( 43.99999999999999289, 50.99999999999999289, 0.000000000000000000 ) ) ;
#18719 = DIRECTION ( 'NONE',  ( -1.000000000000000000, -1.224606353822377258E-16, -0.000000000000000000 ) ) ;
#18720 = LINE ( 'NONE', #14572, #15815 ) ;
#18721 = ORIENTED_EDGE ( 'NONE', *, *, #13447, .F. ) ;
#18722 = ORIENTED_EDGE ( 'NONE', *, *, #7860, .F. ) ;
#18723 = CARTESIAN_POINT ( 'NONE',  ( 6.222797240145152671E-13, -9.127583699786111282, 4.133165578109187166 ) ) ;
#18724 = ORIENTED_EDGE ( 'NONE', *, *, #15855, .F. ) ;
#18725 = APPLICATION_PROTOCOL_DEFINITION ( 'draft international standard', 'automotive_design', 1998, #3096 ) ;
#18726 = ADVANCED_FACE ( 'NONE', ( #12324 ), #6845, .T. ) ;
#18727 = ORIENTED_EDGE ( 'NONE', *, *, #10473, .F. ) ;
#18728 = ORIENTED_EDGE ( 'NONE', *, *, #15421, .T. ) ;
#18729 = DIRECTION ( 'NONE',  ( -1.000000000000000000, -1.224606353822377258E-16, -0.000000000000000000 ) ) ;
#18730 = CARTESIAN_POINT ( 'NONE',  ( 8.680847955711199049, -2.820578480813074496, -12.53316557810918752 ) ) ;
#18731 =( BOUNDED_CURVE ( )  B_SPLINE_CURVE ( 2, ( #11941, #8530, #17442, #13658, #8276, #6477, #19155, #21096, #11684, #21606, #17823 ),
 .UNSPECIFIED., .F., .T. ) 
 B_SPLINE_CURVE_WITH_KNOTS ( ( 3, 2, 2, 2, 2, 3 ),
 ( 0.5000000000000000000, 0.5200000000000000178, 0.5400000000000000355, 0.5600000000000001643, 0.5800000000000000711, 0.6000000000000000888 ),
 .UNSPECIFIED. ) 
 CURVE ( )  GEOMETRIC_REPRESENTATION_ITEM ( )  RATIONAL_B_SPLINE_CURVE ( ( 1.000000000000000000, 0.9510565162951535312, 1.000000000000000000, 0.9510565162951535312, 1.000000000000000000, 0.9510565162951535312, 1.000000000000000000, 0.9510565162951535312, 1.000000000000000000, 0.9510565162951533091, 1.000000000000000222 ) ) 
 REPRESENTATION_ITEM ( '' )  );
#18732 = MECHANICAL_DESIGN_GEOMETRIC_PRESENTATION_REPRESENTATION (  '', ( #10923 ), #11300 ) ;
#18733 = VERTEX_POINT ( 'NONE', #23332 ) ;
#18734 = CARTESIAN_POINT ( 'NONE',  ( -20.99999999999999645, -29.49999999999999645, 11.50000000000000000 ) ) ;
#18735 = DIRECTION ( 'NONE',  ( -1.000000000000000000, 0.000000000000000000, 0.000000000000000000 ) ) ;
#18736 = PRODUCT_DEFINITION_SHAPE ( 'NONE', 'NONE',  #24102 ) ;
#18737 = EDGE_CURVE ( 'NONE', #13688, #588, #14041, .T. ) ;
#18738 = EDGE_CURVE ( 'NONE', #12662, #1759, #15983, .T. ) ;
#18739 = DIRECTION ( 'NONE',  ( 0.000000000000000000, 0.000000000000000000, 1.000000000000000000 ) ) ;
#18740 = ORIENTED_EDGE ( 'NONE', *, *, #9148, .F. ) ;
#18741 = CARTESIAN_POINT ( 'NONE',  ( -20.85000000000000497, 15.03999999999999915, 2.200000000000000178 ) ) ;
#18742 = EDGE_LOOP ( 'NONE', ( #15448, #5643, #23727, #90 ) ) ;
#18743 = ORIENTED_EDGE ( 'NONE', *, *, #10651, .F. ) ;
#18744 = CARTESIAN_POINT ( 'NONE',  ( 0.000000000000000000, 0.000000000000000000, 0.000000000000000000 ) ) ;
#18745 = DIRECTION ( 'NONE',  ( -0.8757121056631633760, -0.4828336235133056653, 1.675165643398955870E-15 ) ) ;
#18746 = CARTESIAN_POINT ( 'NONE',  ( 78.94340820527399671, 7.562528597612068045E-15, 0.000000000000000000 ) ) ;
#18747 = CARTESIAN_POINT ( 'NONE',  ( -20.85000000000000497, 15.03999999999999915, 2.200000000000000178 ) ) ;
#18748 = CARTESIAN_POINT ( 'NONE',  ( 9.500000000000000000, 6.470877716354879437E-13, -6.059589141758143782 ) ) ;
#18749 = FACE_OUTER_BOUND ( 'NONE', #4693, .T. ) ;
#18750 = CARTESIAN_POINT ( 'NONE',  ( 40.66734255040735491, -26.56420859267090862, -1.500000000000000000 ) ) ;
#18751 = ORIENTED_EDGE ( 'NONE', *, *, #7438, .F. ) ;
#18752 = EDGE_LOOP ( 'NONE', ( #3489, #7076, #17814, #2282 ) ) ;
#18753 = VECTOR ( 'NONE', #10240, 1000.000000000000000 ) ;
#18754 = ORIENTED_EDGE ( 'NONE', *, *, #5308, .F. ) ;
#18755 = ORIENTED_EDGE ( 'NONE', *, *, #20421, .F. ) ;
#18756 = DIRECTION ( 'NONE',  ( 0.000000000000000000, -1.000000000000000000, 0.000000000000000000 ) ) ;
#18757 = LINE ( 'NONE', #18295, #13379 ) ;
#18758 = DIRECTION ( 'NONE',  ( -0.000000000000000000, -0.000000000000000000, -1.000000000000000000 ) ) ;
#18759 = FILL_AREA_STYLE_COLOUR ( '', #1761 ) ;
#18760 = CARTESIAN_POINT ( 'NONE',  ( 2.454813078130514813E-15, 16.67999999999999972, 13.00000000000000178 ) ) ;
#18761 = EDGE_CURVE ( 'NONE', #3993, #22463, #14451, .T. ) ;
#18762 = ORIENTED_EDGE ( 'NONE', *, *, #22243, .F. ) ;
#18763 = AXIS2_PLACEMENT_3D ( 'NONE', #725, #12036, #9967 ) ;
#18764 = AXIS2_PLACEMENT_3D ( 'NONE', #19791, #13093, #20662 ) ;
#18765 = CARTESIAN_POINT ( 'NONE',  ( 9.000000000000000000, 1.102182119232617714E-15, 0.9999999999999731326 ) ) ;
#18766 = CARTESIAN_POINT ( 'NONE',  ( -41.00000000000000000, -6.000000000000000888, 11.00000000000000000 ) ) ;
#18767 = DIRECTION ( 'NONE',  ( -0.000000000000000000, -0.000000000000000000, -1.000000000000000000 ) ) ;
#18768 = CIRCLE ( 'NONE', #10187, 1.000000000000000888 ) ;
#18769 = CARTESIAN_POINT ( 'NONE',  ( -16.82499651802898200, 7.532250541895348483, 5.808290850931494553 ) ) ;
#18770 = LINE ( 'NONE', #11563, #11043 ) ;
#18771 = VERTEX_POINT ( 'NONE', #21735 ) ;
#18772 = LINE ( 'NONE', #5848, #23618 ) ;
#18773 = ORIENTED_EDGE ( 'NONE', *, *, #19488, .T. ) ;
#18774 = CARTESIAN_POINT ( 'NONE',  ( 77.78386452199872281, -9.244463733058732095E-30, 5.000000000000007994 ) ) ;
#18775 = ORIENTED_EDGE ( 'NONE', *, *, #13568, .T. ) ;
#18776 = DIRECTION ( 'NONE',  ( 1.000000000000000000, 0.000000000000000000, 0.000000000000000000 ) ) ;
#18777 = EDGE_CURVE ( 'NONE', #2222, #2505, #57, .T. ) ;
#18778 = ORIENTED_EDGE ( 'NONE', *, *, #17652, .F. ) ;
#18779 = CARTESIAN_POINT ( 'NONE',  ( 17.25000000000000000, 15.50000000000000178, 16.70000000000000284 ) ) ;
#18780 = DIRECTION ( 'NONE',  ( -1.000000000000000000, 0.000000000000000000, 0.000000000000000000 ) ) ;
#18781 = AXIS2_PLACEMENT_3D ( 'NONE', #2274, #20694, #9332 ) ;
#18782 = CARTESIAN_POINT ( 'NONE',  ( 0.000000000000000000, 0.000000000000000000, 4.000000000000000000 ) ) ;
#18783 = AXIS2_PLACEMENT_3D ( 'NONE', #2576, #6110, #6482 ) ;
#18784 = ADVANCED_FACE ( 'NONE', ( #17450 ), #23069, .F. ) ;
#18785 = TOROIDAL_SURFACE ( 'NONE', #18802, 5.400000000000001243, 0.4000000000000000222 ) ;
#18786 = CIRCLE ( 'NONE', #23858, 9.499999999999998224 ) ;
#18787 = DIRECTION ( 'NONE',  ( 1.000000000000000000, 0.000000000000000000, -0.000000000000000000 ) ) ;
#18788 = CONICAL_SURFACE ( 'NONE', #7100, 5.000000000000007994, 0.9599310885968855844 ) ;
#18789 = AXIS2_PLACEMENT_3D ( 'NONE', #15638, #4580, #23604 ) ;
#18790 = ADVANCED_FACE ( 'NONE', ( #9008 ), #18195, .T. ) ;
#18791 = CIRCLE ( 'NONE', #8261, 1.500000000000001332 ) ;
#18792 = EDGE_CURVE ( 'NONE', #9278, #17662, #5481, .T. ) ;
#18793 = DIRECTION ( 'NONE',  ( -0.1039766011667100087, 0.9945797436152714610, 0.000000000000000000 ) ) ;
#18794 = CARTESIAN_POINT ( 'NONE',  ( -9.500000000000211386, 3.086737114211961064, -8.959589141758140585 ) ) ;
#18795 = ORIENTED_EDGE ( 'NONE', *, *, #5797, .T. ) ;
#18796 = DIRECTION ( 'NONE',  ( -0.000000000000000000, -0.000000000000000000, 1.000000000000000000 ) ) ;
#18797 = ORIENTED_EDGE ( 'NONE', *, *, #11117, .F. ) ;
#18798 = CARTESIAN_POINT ( 'NONE',  ( 23.00000000000000000, -10.66755332433025139, 4.772587172891002538 ) ) ;
#18799 = CARTESIAN_POINT ( 'NONE',  ( 40.00000000000000000, -27.79189783386526358, 27.00000000000000000 ) ) ;
#18800 = CARTESIAN_POINT ( 'NONE',  ( -14.99999999999999645, 15.50000000000000178, 16.70000000000000284 ) ) ;
#18801 = CARTESIAN_POINT ( 'NONE',  ( 23.00000000000000000, 0.000000000000000000, 0.000000000000000000 ) ) ;
#18802 = AXIS2_PLACEMENT_3D ( 'NONE', #5749, #15107, #18923 ) ;
#18803 = LINE ( 'NONE', #22962, #10479 ) ;
#18804 = FACE_OUTER_BOUND ( 'NONE', #21026, .T. ) ;
#18805 = AXIS2_PLACEMENT_3D ( 'NONE', #14970, #14849, #22318 ) ;
#18806 = DIRECTION ( 'NONE',  ( 0.000000000000000000, -1.000000000000000000, 0.000000000000000000 ) ) ;
#18807 = VECTOR ( 'NONE', #13563, 1000.000000000000000 ) ;
#18808 = CARTESIAN_POINT ( 'NONE',  ( 5.000000000000000000, 4.685197434473818312, -1.301042606982605321E-15 ) ) ;
#18809 = ORIENTED_EDGE ( 'NONE', *, *, #2845, .F. ) ;
#18810 = AXIS2_PLACEMENT_3D ( 'NONE', #5620, #11078, #18776 ) ;
#18811 = CARTESIAN_POINT ( 'NONE',  ( 63.81818181818181301, 4.172000000000015696, 5.109226446042767468E-16 ) ) ;
#18812 = PRODUCT_DEFINITION_SHAPE ( 'NONE', 'NONE',  #24121 ) ;
#18813 = FACE_OUTER_BOUND ( 'NONE', #5384, .T. ) ;
#18814 = CONICAL_SURFACE ( 'NONE', #5967, 2.024999999999999911, 0.7853981633974222998 ) ;
#18815 = DIRECTION ( 'NONE',  ( -1.000000000000000000, 0.000000000000000000, 0.000000000000000000 ) ) ;
#18816 = FACE_OUTER_BOUND ( 'NONE', #4040, .T. ) ;
#18817 = EDGE_LOOP ( 'NONE', ( #15265, #17107, #23720, #4449 ) ) ;
#18818 = ADVANCED_FACE ( 'NONE', ( #3652 ), #8895, .F. ) ;
#18819 = ADVANCED_FACE ( 'NONE', ( #20147, #6962 ), #11064, .T. ) ;
#18820 = VERTEX_POINT ( 'NONE', #1588 ) ;
#18821 = AXIS2_PLACEMENT_3D ( 'NONE', #21897, #15117, #2211 ) ;
#18822 = ORIENTED_EDGE ( 'NONE', *, *, #8671, .F. ) ;
#18824 = AXIS2_PLACEMENT_3D ( 'NONE', #13533, #11670, #2786 ) ;
#18823 = DIRECTION ( 'NONE',  ( 0.000000000000000000, 0.000000000000000000, 1.000000000000000000 ) ) ;
#18825 = CONICAL_SURFACE ( 'NONE', #3243, 4.172000000000008590, 0.9599310885968742602 ) ;
#18826 = VECTOR ( 'NONE', #5680, 1000.000000000000000 ) ;
#18827 = DIRECTION ( 'NONE',  ( 1.000000000000000000, 0.000000000000000000, 0.000000000000000000 ) ) ;
#18828 = VERTEX_POINT ( 'NONE', #1362 ) ;
#18829 = VECTOR ( 'NONE', #3558, 1000.000000000000000 ) ;
#18830 = DIRECTION ( 'NONE',  ( -0.000000000000000000, 0.000000000000000000, 1.000000000000000000 ) ) ;
#18831 = CARTESIAN_POINT ( 'NONE',  ( 0.000000000000000000, 0.000000000000000000, -1.500000000000000000 ) ) ;
#18832 = VECTOR ( 'NONE', #854, 1000.000000000000114 ) ;
#18833 = ORIENTED_EDGE ( 'NONE', *, *, #7253, .F. ) ;
#18834 = CARTESIAN_POINT ( 'NONE',  ( -7.485396084480734125, -5.856027100821079578, -3.500200866489544538 ) ) ;
#18835 =( REPRESENTATION_RELATIONSHIP ('NONE','NONE', #21748, #15290 ) REPRESENTATION_RELATIONSHIP_WITH_TRANSFORMATION ( #9651 )SHAPE_REPRESENTATION_RELATIONSHIP( ) );
#18836 = ORIENTED_EDGE ( 'NONE', *, *, #9705, .F. ) ;
#18837 = DIRECTION ( 'NONE',  ( 0.000000000000000000, 0.000000000000000000, 1.000000000000000000 ) ) ;
#18838 = DIRECTION ( 'NONE',  ( -0.000000000000000000, -0.000000000000000000, 1.000000000000000000 ) ) ;
#18839 = CARTESIAN_POINT ( 'NONE',  ( 9.500000000000000000, 6.470877716354879437E-13, 11.20674201446023410 ) ) ;
#18840 = ORIENTED_EDGE ( 'NONE', *, *, #5929, .F. ) ;
#18841 = CONICAL_SURFACE ( 'NONE', #8311, 4.172000000000008590, 0.9599310885968742602 ) ;
#18842 = DIRECTION ( 'NONE',  ( -0.000000000000000000, 0.000000000000000000, 1.000000000000000000 ) ) ;
#18843 = DIRECTION ( 'NONE',  ( 0.8298699724180969017, -0.5579568342432840167, 0.000000000000000000 ) ) ;
#18844 = ORIENTED_EDGE ( 'NONE', *, *, #10628, .T. ) ;
#18845 = CIRCLE ( 'NONE', #8314, 5.099999999999996980 ) ;
#18846 = EDGE_LOOP ( 'NONE', ( #9018, #10635, #72 ) ) ;
#18847 = CARTESIAN_POINT ( 'NONE',  ( -7.022953521755574080, 5.102474405759713783, 5.433165578109188765 ) ) ;
#18848 = ORIENTED_EDGE ( 'NONE', *, *, #14030, .F. ) ;
#18849 = CIRCLE ( 'NONE', #4441, 5.000000000000007994 ) ;
#18850 = EDGE_CURVE ( 'NONE', #3750, #17649, #21499, .T. ) ;
#18851 = VECTOR ( 'NONE', #7015, 1000.000000000000000 ) ;
#18852 = EDGE_CURVE ( 'NONE', #22152, #14068, #5251, .T. ) ;
#18853 = CIRCLE ( 'NONE', #23557, 5.000000000000007994 ) ;
#18854 = PRODUCT_CONTEXT ( 'NONE', #12741, 'mechanical' ) ;
#18855 = VECTOR ( 'NONE', #23309, 1000.000000000000000 ) ;
#18856 = VERTEX_POINT ( 'NONE', #14386 ) ;
#18857 = ORIENTED_EDGE ( 'NONE', *, *, #17974, .T. ) ;
#18858 = FACE_OUTER_BOUND ( 'NONE', #15478, .T. ) ;
#18859 = CARTESIAN_POINT ( 'NONE',  ( -7.022953521754877748, -5.102474405760673015, -11.83316557810918823 ) ) ;
#18860 = EDGE_LOOP ( 'NONE', ( #18351, #7433, #6428, #203, #9922 ) ) ;
#18861 = LINE ( 'NONE', #22531, #944 ) ;
#18862 = CARTESIAN_POINT ( 'NONE',  ( 17.25000000000000000, 15.50000000000000178, 7.700000000000001954 ) ) ;
#18863 = DIRECTION ( 'NONE',  ( 0.000000000000000000, -1.000000000000000000, 0.000000000000000000 ) ) ;
#18864 = CYLINDRICAL_SURFACE ( 'NONE', #20201, 2.000000000000000000 ) ;
#18865 = DIRECTION ( 'NONE',  ( -1.000000000000000000, -1.224606353822377258E-16, -0.000000000000000000 ) ) ;
#18866 = CIRCLE ( 'NONE', #7179, 1.000000000000001998 ) ;
#18867 = VECTOR ( 'NONE', #5162, 1000.000000000000000 ) ;
#18868 = VERTEX_POINT ( 'NONE', #16338 ) ;
#18869 = CIRCLE ( 'NONE', #10294, 1.999999999999997113 ) ;
#18870 = CARTESIAN_POINT ( 'NONE',  ( 0.000000000000000000, 0.000000000000000000, 0.4999999999999970024 ) ) ;
#18871 = FACE_OUTER_BOUND ( 'NONE', #20620, .T. ) ;
#18872 = AXIS2_PLACEMENT_3D ( 'NONE', #1059, #15924, #12253 ) ;
#18873 = DIRECTION ( 'NONE',  ( -0.000000000000000000, 0.000000000000000000, -1.000000000000000000 ) ) ;
#18874 = CARTESIAN_POINT ( 'NONE',  ( 1.999999999999994449, -45.00000000000000000, -27.00000000000000000 ) ) ;
#18875 = EDGE_CURVE ( 'NONE', #21660, #6981, #15618, .T. ) ;
#18876 = CIRCLE ( 'NONE', #15772, 1.999999999999994449 ) ;
#18877 = DIRECTION ( 'NONE',  ( 0.000000000000000000, -1.000000000000000000, 0.000000000000000000 ) ) ;
#18878 = DIRECTION ( 'NONE',  ( -1.000000000000000000, 0.000000000000000000, 0.000000000000000000 ) ) ;
#18879 = CARTESIAN_POINT ( 'NONE',  ( -9.499999999999786837, -3.086737114213265354, 8.306742014460233747 ) ) ;
#18880 = ORIENTED_EDGE ( 'NONE', *, *, #4708, .F. ) ;
#18881 = ORIENTED_EDGE ( 'NONE', *, *, #476, .T. ) ;
#18882 = EDGE_CURVE ( 'NONE', #9290, #17358, #20255, .T. ) ;
#18883 = VERTEX_POINT ( 'NONE', #5025 ) ;
#18884 = ADVANCED_FACE ( 'NONE', ( #14853, #3420 ), #20367, .F. ) ;
#18885 = ORIENTED_EDGE ( 'NONE', *, *, #19333, .T. ) ;
#18886 =( BOUNDED_CURVE ( )  B_SPLINE_CURVE ( 2, ( #18748, #15312, #2027, #19116, #7997, #5817, #2160, #13244, #2390, #15445, #9807 ),
 .UNSPECIFIED., .F., .T. ) 
 B_SPLINE_CURVE_WITH_KNOTS ( ( 3, 2, 2, 2, 2, 3 ),
 ( 0.6000000000000000888, 0.6200000000000001066, 0.6400000000000001243, 0.6600000000000001421, 0.6800000000000001599, 0.7000000000000000666 ),
 .UNSPECIFIED. ) 
 CURVE ( )  GEOMETRIC_REPRESENTATION_ITEM ( )  RATIONAL_B_SPLINE_CURVE ( ( 0.9999999999999997780, 0.9510565162951537532, 1.000000000000000000, 0.9510565162951535312, 1.000000000000000000, 0.9510565162951535312, 1.000000000000000000, 0.9510565162951535312, 1.000000000000000000, 0.9510565162951533091, 1.000000000000000222 ) ) 
 REPRESENTATION_ITEM ( '' )  );
#18887 = AXIS2_PLACEMENT_3D ( 'NONE', #11186, #23917, #16582 ) ;
#18888 = CARTESIAN_POINT ( 'NONE',  ( 29.00000000000000000, -29.50000000000000355, 11.50000000000000000 ) ) ;
#18889 = DIRECTION ( 'NONE',  ( 0.000000000000000000, 0.000000000000000000, 1.000000000000000000 ) ) ;
#18890 = UNCERTAINTY_MEASURE_WITH_UNIT (LENGTH_MEASURE( 1.000000000000000082E-05 ), #17818, 'distance_accuracy_value', 'NONE');
#18891 = VECTOR ( 'NONE', #9587, 1000.000000000000114 ) ;
#18892 = MANIFOLD_SOLID_BREP ( 'Revolve1', #17899 ) ;
#18893 = AXIS2_PLACEMENT_3D ( 'NONE', #8553, #5910, #4927 ) ;
#18894 = DIRECTION ( 'NONE',  ( 1.000000000000000000, 0.000000000000000000, 0.000000000000000000 ) ) ;
#18895 = CARTESIAN_POINT ( 'NONE',  ( -31.74999999999995737, 0.000000000000000000, 0.000000000000000000 ) ) ;
#18896 = FACE_BOUND ( 'NONE', #10965, .T. ) ;
#18897 = CARTESIAN_POINT ( 'NONE',  ( -40.89823313241237912, -26.41789760203349502, 27.00000000000000000 ) ) ;
#18898 = AXIS2_PLACEMENT_3D ( 'NONE', #4132, #11911, #20710 ) ;
#18899 = FACE_OUTER_BOUND ( 'NONE', #23356, .T. ) ;
#18900 = VERTEX_POINT ( 'NONE', #22810 ) ;
#18901 = DIRECTION ( 'NONE',  ( -0.000000000000000000, -0.000000000000000000, -1.000000000000000000 ) ) ;
#18902 = PRESENTATION_STYLE_ASSIGNMENT (( #15096 ) ) ;
#18903 = LINE ( 'NONE', #607, #23491 ) ;
#18904 = CARTESIAN_POINT ( 'NONE',  ( 84.18181818181818699, 7.491529369508391930E-15, 0.000000000000000000 ) ) ;
#18905 = EDGE_CURVE ( 'NONE', #15347, #11492, #11327, .T. ) ;
#18906 = DIRECTION ( 'NONE',  ( 0.000000000000000000, 0.000000000000000000, 1.000000000000000000 ) ) ;
#18907 = ORIENTED_EDGE ( 'NONE', *, *, #20076, .F. ) ;
#18908 = TOROIDAL_SURFACE ( 'NONE', #13510, 2.500000000000001776, 1.000000000000000000 ) ;
#18909 = CARTESIAN_POINT ( 'NONE',  ( 68.76159002345582394, 7.562528597612068045E-15, 0.000000000000000000 ) ) ;
#18910 = ORIENTED_EDGE ( 'NONE', *, *, #22646, .F. ) ;
#18911 = FACE_OUTER_BOUND ( 'NONE', #15826, .T. ) ;
#18912 = VECTOR ( 'NONE', #20809, 1000.000000000000000 ) ;
#18913 = ORIENTED_EDGE ( 'NONE', *, *, #11707, .T. ) ;
#18914 = DIRECTION ( 'NONE',  ( -1.000000000000000000, -1.224606353822377258E-16, -0.000000000000000000 ) ) ;
#18916 = ADVANCED_FACE ( 'NONE', ( #122 ), #15338, .T. ) ;
#18915 = AXIS2_PLACEMENT_3D ( 'NONE', #1478, #8890, #16327 ) ;
#18917 = ORIENTED_EDGE ( 'NONE', *, *, #4742, .T. ) ;
#18918 = DIRECTION ( 'NONE',  ( 1.000000000000000000, 0.000000000000000000, 0.000000000000000000 ) ) ;
#18920 = EDGE_CURVE ( 'NONE', #7541, #2619, #355, .T. ) ;
#18919 = CIRCLE ( 'NONE', #21257, 18.50000000000000000 ) ;
#18921 = ADVANCED_BREP_SHAPE_REPRESENTATION ( '', ( #2159, #8005 ), #12698 ) ;
#18922 = CARTESIAN_POINT ( 'NONE',  ( 0.000000000000000000, 12.02595010061954461, 13.22467954916291433 ) ) ;
#18923 = DIRECTION ( 'NONE',  ( 0.000000000000000000, 0.000000000000000000, -1.000000000000000000 ) ) ;
#18924 = CARTESIAN_POINT ( 'NONE',  ( 41.73082370883260239, 27.62204025492843940, -3.000000000000000000 ) ) ;
#18925 = DIRECTION ( 'NONE',  ( -4.613626265895764052E-16, 1.000000000000000000, 0.000000000000000000 ) ) ;
#18926 = DIRECTION ( 'NONE',  ( -0.000000000000000000, -0.000000000000000000, -1.000000000000000000 ) ) ;
#18927 = CARTESIAN_POINT ( 'NONE',  ( 5.871322893124553133, -8.081182679343980269, -3.759589141758144404 ) ) ;
#18928 = VERTEX_POINT ( 'NONE', #20492 ) ;
#18929 = DIRECTION ( 'NONE',  ( -0.000000000000000000, -0.000000000000000000, -1.000000000000000000 ) ) ;
#18930 = EDGE_CURVE ( 'NONE', #1666, #17534, #853, .T. ) ;
#18931 = AXIS2_PLACEMENT_3D ( 'NONE', #11007, #22040, #1772 ) ;
#18932 = ORIENTED_EDGE ( 'NONE', *, *, #2348, .T. ) ;
#18933 = CARTESIAN_POINT ( 'NONE',  ( 5.871322893123448239, 8.081182679344781405, 5.506742014460233925 ) ) ;
#18934 = CARTESIAN_POINT ( 'NONE',  ( 2.693550685028764491, 8.587845621821196929, 79.66457110399080932 ) ) ;
#18935 = FACE_BOUND ( 'NONE', #15672, .T. ) ;
#18936 = DIRECTION ( 'NONE',  ( 0.000000000000000000, 0.000000000000000000, 1.000000000000000000 ) ) ;
#18937 = ADVANCED_FACE ( 'NONE', ( #1935 ), #22559, .F. ) ;
#18938 = DIRECTION ( 'NONE',  ( 0.000000000000000000, 0.7557495743542552713, 0.6548607339452886533 ) ) ;
#18939 = DIRECTION ( 'NONE',  ( 0.000000000000000000, -0.9898214418809342385, 0.1423148382732755957 ) ) ;
#18940 = DIRECTION ( 'NONE',  ( -0.000000000000000000, -0.000000000000000000, -1.000000000000000000 ) ) ;
#18941 = DIRECTION ( 'NONE',  ( 0.000000000000000000, 0.000000000000000000, 1.000000000000000000 ) ) ;
#18942 = VERTEX_POINT ( 'NONE', #13148 ) ;
#18943 = CARTESIAN_POINT ( 'NONE',  ( 23.00000000000000000, 12.00453763395396756, -7.608955687739546114 ) ) ;
#18944 = EDGE_CURVE ( 'NONE', #14507, #2676, #9383, .T. ) ;
#18945 = CARTESIAN_POINT ( 'NONE',  ( 5.365059087799947335, -7.384370330706356178, 10.33316557810918823 ) ) ;
#18946 = AXIS2_PLACEMENT_3D ( 'NONE', #14714, #12639, #20107 ) ;
#18947 = EDGE_CURVE ( 'NONE', #5147, #12646, #15240, .T. ) ;
#18948 = DIRECTION ( 'NONE',  ( -1.000000000000000000, 0.000000000000000000, 0.000000000000000000 ) ) ;
#18949 = AXIS2_PLACEMENT_3D ( 'NONE', #23860, #4733, #1082 ) ;
#18950 = DIRECTION ( 'NONE',  ( 0.000000000000000000, 0.000000000000000000, 1.000000000000000000 ) ) ;
#18951 = VERTEX_POINT ( 'NONE', #20723 ) ;
#18952 = AXIS2_PLACEMENT_3D ( 'NONE', #23898, #18047, #14613 ) ;
#18953 = AXIS2_PLACEMENT_3D ( 'NONE', #4772, #8780, #12186 ) ;
#18954 = ORIENTED_EDGE ( 'NONE', *, *, #10147, .T. ) ;
#18955 = ITEM_DEFINED_TRANSFORMATION ( 'NONE', 'NONE', #17787,  #8005 ) ;
#18956 = ORIENTED_EDGE ( 'NONE', *, *, #8879, .F. ) ;
#18957 = FACE_OUTER_BOUND ( 'NONE', #19187, .T. ) ;
#18958 = LINE ( 'NONE', #51, #8682 ) ;
#18959 = ORIENTED_EDGE ( 'NONE', *, *, #299, .F. ) ;
#18960 = ORIENTED_EDGE ( 'NONE', *, *, #12494, .T. ) ;
#18961 = EDGE_CURVE ( 'NONE', #12158, #16948, #467, .T. ) ;
#18962 = CONICAL_SURFACE ( 'NONE', #23264, 5.000000000000007994, 0.9599310885968855844 ) ;
#18963 = DIRECTION ( 'NONE',  ( -1.000000000000000000, 0.000000000000000000, 0.000000000000000000 ) ) ;
#18964 = ORIENTED_EDGE ( 'NONE', *, *, #13807, .T. ) ;
#18965 = FACE_OUTER_BOUND ( 'NONE', #7833, .T. ) ;
#18966 = AXIS2_PLACEMENT_3D ( 'NONE', #16025, #23490, #8831 ) ;
#18967 = EDGE_CURVE ( 'NONE', #15320, #13734, #2002, .T. ) ;
#18968 = ORIENTED_EDGE ( 'NONE', *, *, #4157, .F. ) ;
#18969 = DIRECTION ( 'NONE',  ( -1.000000000000000000, -1.224606353822377258E-16, -0.000000000000000000 ) ) ;
#18970 = CARTESIAN_POINT ( 'NONE',  ( 40.66734255040736201, -26.56420859267091217, -3.000000000000000000 ) ) ;
#18971 = CIRCLE ( 'NONE', #1004, 1.500000000000001332 ) ;
#18972 = DIRECTION ( 'NONE',  ( 1.000000000000000000, 6.811450227741984732E-14, -0.000000000000000000 ) ) ;
#18973 = CYLINDRICAL_SURFACE ( 'NONE', #5634, 1.000000000000000888 ) ;
#18974 = ORIENTED_EDGE ( 'NONE', *, *, #17024, .F. ) ;
#18975 = DIRECTION ( 'NONE',  ( 0.000000000000000000, 0.000000000000000000, 1.000000000000000000 ) ) ;
#18976 = DIRECTION ( 'NONE',  ( -1.000000000000000000, 0.000000000000000000, -0.000000000000000000 ) ) ;
#18977 = CYLINDRICAL_SURFACE ( 'NONE', #20890, 5.099999999999996980 ) ;
#18978 = ORIENTED_EDGE ( 'NONE', *, *, #9876, .F. ) ;
#18979 = VECTOR ( 'NONE', #23840, 1000.000000000000000 ) ;
#18980 = ORIENTED_EDGE ( 'NONE', *, *, #7021, .T. ) ;
#18981 = CARTESIAN_POINT ( 'NONE',  ( 2.682529543899157876, 8.255977015246598327, 7.033165578109189298 ) ) ;
#18982 = ORIENTED_EDGE ( 'NONE', *, *, #12519, .F. ) ;
#18983 = ORIENTED_EDGE ( 'NONE', *, *, #22382, .F. ) ;
#18984 = AXIS2_PLACEMENT_3D ( 'NONE', #8665, #4925, #12338 ) ;
#18985 = DIRECTION ( 'NONE',  ( 0.000000000000000000, 0.000000000000000000, 1.000000000000000000 ) ) ;
#18986 = VERTEX_POINT ( 'NONE', #19136 ) ;
#18987 = EDGE_LOOP ( 'NONE', ( #12860, #19854, #2193, #7601 ) ) ;
#18988 = DIRECTION ( 'NONE',  ( -1.000000000000000000, 0.000000000000000000, 0.000000000000000000 ) ) ;
#18989 = ORIENTED_EDGE ( 'NONE', *, *, #6076, .T. ) ;
#18990 = CARTESIAN_POINT ( 'NONE',  ( -29.00000000000000000, -29.49999999999999645, 11.50000000000000000 ) ) ;
#18991 = DIRECTION ( 'NONE',  ( -0.000000000000000000, -0.000000000000000000, -1.000000000000000000 ) ) ;
#18993 = DIRECTION ( 'NONE',  ( 1.000000000000000000, -0.000000000000000000, -0.000000000000000000 ) ) ;
#18992 = APPLICATION_CONTEXT ( 'automotive_design' ) ;
#18994 = DIRECTION ( 'NONE',  ( -0.000000000000000000, -0.000000000000000000, 1.000000000000000000 ) ) ;
#18995 = LINE ( 'NONE', #11153, #13968 ) ;
#18996 = ORIENTED_EDGE ( 'NONE', *, *, #12137, .F. ) ;
#18997 = DIRECTION ( 'NONE',  ( 1.000000000000000000, 0.000000000000000000, 0.000000000000000000 ) ) ;
#18998 = ADVANCED_FACE ( 'NONE', ( #3778 ), #23838, .F. ) ;
#18999 = EDGE_CURVE ( 'NONE', #13326, #4606, #20720, .T. ) ;
#19000 = ORIENTED_EDGE ( 'NONE', *, *, #2679, .T. ) ;
#19001 = DIRECTION ( 'NONE',  ( 0.000000000000000000, -1.000000000000000000, 0.000000000000000000 ) ) ;
#19002 = CARTESIAN_POINT ( 'NONE',  ( -30.32370777929699202, 42.16181938034195298, 0.000000000000000000 ) ) ;
#19003 = DIRECTION ( 'NONE',  ( 1.000000000000000000, 1.224606353822377258E-16, 0.000000000000000000 ) ) ;
#19004 = CYLINDRICAL_SURFACE ( 'NONE', #8744, 17.87500000001787726 ) ;
#19005 = CARTESIAN_POINT ( 'NONE',  ( 0.000000000000000000, 0.000000000000000000, 0.000000000000000000 ) ) ;
#19006 = CARTESIAN_POINT ( 'NONE',  ( 90.00000000000000000, 0.000000000000000000, 0.000000000000000000 ) ) ;
#19007 = CYLINDRICAL_SURFACE ( 'NONE', #16765, 11.00000000000000355 ) ;
#19008 = VERTEX_POINT ( 'NONE', #22326 ) ;
#19009 = VERTEX_POINT ( 'NONE', #14978 ) ;
#19010 = CARTESIAN_POINT ( 'NONE',  ( 8.680847955711199049, -2.820578480813074496, 12.53316557810918752 ) ) ;
#19011 = AXIS2_PLACEMENT_3D ( 'NONE', #778, #4446, #8070 ) ;
#19012 = VERTEX_POINT ( 'NONE', #9609 ) ;
#19013 = CARTESIAN_POINT ( 'NONE',  ( 693.7625826937756983, 903.2366700927681222, 1347.481724745927977 ) ) ;
#19014 = ORIENTED_EDGE ( 'NONE', *, *, #6984, .T. ) ;
#19015 = CARTESIAN_POINT ( 'NONE',  ( 20.85000000000000497, 16.67999999999999972, 13.50000000000000178 ) ) ;
#19016 = AXIS2_PLACEMENT_3D ( 'NONE', #5807, #13233, #10802 ) ;
#19017 = MANIFOLD_SOLID_BREP ( 'Chamfer1', #15515 ) ;
#19018 = ADVANCED_FACE ( 'NONE', ( #17538 ), #76, .T. ) ;
#19019 = CYLINDRICAL_SURFACE ( 'NONE', #23155, 5.100000000000000533 ) ;
#19020 = CARTESIAN_POINT ( 'NONE',  ( 87.96568270381690979, 7.420530141404717394E-15, 0.000000000000000000 ) ) ;
#19021 = DIRECTION ( 'NONE',  ( -1.000000000000000000, -1.224606353822377258E-16, -0.000000000000000000 ) ) ;
#19022 = DIRECTION ( 'NONE',  ( -0.000000000000000000, -0.000000000000000000, -1.000000000000000000 ) ) ;
#19023 = ORIENTED_EDGE ( 'NONE', *, *, #13955, .T. ) ;
#19024 = EDGE_CURVE ( 'NONE', #3297, #13594, #1249, .T. ) ;
#19025 = DIRECTION ( 'NONE',  ( 1.000000000000000000, 1.224606353822377258E-16, 0.000000000000000000 ) ) ;
#19026 = EDGE_CURVE ( 'NONE', #10133, #17959, #13694, .T. ) ;
#19027 = FACE_OUTER_BOUND ( 'NONE', #12303, .T. ) ;
#19028 = EDGE_CURVE ( 'NONE', #12778, #16881, #16049, .T. ) ;
#19029 = DIRECTION ( 'NONE',  ( 0.000000000000000000, 0.000000000000000000, 1.000000000000000000 ) ) ;
#19030 = DIRECTION ( 'NONE',  ( 1.000000000000000000, 1.224606353822377258E-16, 0.000000000000000000 ) ) ;
#19031 = EDGE_CURVE ( 'NONE', #2772, #20942, #21587, .T. ) ;
#19032 = CARTESIAN_POINT ( 'NONE',  ( 2.454813078130514813E-15, -16.67999999999999972, 14.50000000000000000 ) ) ;
#19033 = CARTESIAN_POINT ( 'NONE',  ( -7.685661446561619314, -5.583959896779019161, 4.406742014460233392 ) ) ;
#19034 = ORIENTED_EDGE ( 'NONE', *, *, #13263, .T. ) ;
#19035 = CIRCLE ( 'NONE', #17060, 4.249999999999996447 ) ;
#19036 = DIRECTION ( 'NONE',  ( -0.000000000000000000, -0.000000000000000000, -1.000000000000000000 ) ) ;
#19037 = AXIS2_PLACEMENT_3D ( 'NONE', #18071, #21615, #23569 ) ;
#19038 = EDGE_LOOP ( 'NONE', ( #11278, #20268, #5513, #13061 ) ) ;
#19039 = VERTEX_POINT ( 'NONE', #4879 ) ;
#19040 = FACE_OUTER_BOUND ( 'NONE', #6385, .T. ) ;
#19041 = EDGE_LOOP ( 'NONE', ( #8167, #6142, #3631, #14149, #6782 ) ) ;
#19042 = FACE_OUTER_BOUND ( 'NONE', #18817, .T. ) ;
#19043 = DIRECTION ( 'NONE',  ( -1.000000000000000000, -1.224606353822377258E-16, -0.000000000000000000 ) ) ;
#19044 = DIRECTION ( 'NONE',  ( 1.000000000000000000, 0.000000000000000000, -0.000000000000000000 ) ) ;
#19045 = DIRECTION ( 'NONE',  ( 0.000000000000000000, 0.000000000000000000, 1.000000000000000000 ) ) ;
#19046 = VECTOR ( 'NONE', #2402, 1000.000000000000000 ) ;
#19047 = EDGE_CURVE ( 'NONE', #2378, #8445, #1637, .T. ) ;
#19048 = LINE ( 'NONE', #13921, #10632 ) ;
#19049 = DIRECTION ( 'NONE',  ( -1.000000000000000000, 0.000000000000000000, 0.000000000000000000 ) ) ;
#19050 = DIRECTION ( 'NONE',  ( -1.000000000000000000, -1.224606353822377258E-16, -0.000000000000000000 ) ) ;
#19051 = VERTEX_POINT ( 'NONE', #23417 ) ;
#19052 = DIRECTION ( 'NONE',  ( -0.000000000000000000, -0.000000000000000000, -1.000000000000000000 ) ) ;
#19053 = ADVANCED_FACE ( 'NONE', ( #17427 ), #5528, .T. ) ;
#19054 = ADVANCED_FACE ( 'NONE', ( #8392 ), #18389, .T. ) ;
#19055 = EDGE_LOOP ( 'NONE', ( #2039, #1169, #9690, #680 ) ) ;
#19056 = CARTESIAN_POINT ( 'NONE',  ( -8.354078656939378789, -4.088315676896441708, 12.20717083813929271 ) ) ;
#19057 = CARTESIAN_POINT ( 'NONE',  ( -9.378401895172215674, 3.550564238312661509E-15, 12.12159810482778077 ) ) ;
#19058 = CARTESIAN_POINT ( 'NONE',  ( 43.50000000000000711, 25.84341543330623026, 0.000000000000000000 ) ) ;
#19059 = CARTESIAN_POINT ( 'NONE',  ( 23.00000000000000000, 0.000000000000000000, 0.000000000000000000 ) ) ;
#19060 = AXIS2_PLACEMENT_3D ( 'NONE', #11832, #15493, #5869 ) ;
#19061 = DIRECTION ( 'NONE',  ( -1.000000000000000000, 0.000000000000000000, 0.000000000000000000 ) ) ;
#19062 = CARTESIAN_POINT ( 'NONE',  ( -7.685661446561619314, -5.583959896779019161, -4.406742014460233392 ) ) ;
#19063 = ORIENTED_EDGE ( 'NONE', *, *, #17521, .T. ) ;
#19064 = CARTESIAN_POINT ( 'NONE',  ( -35.99999999999994316, -60.00000000000000000, 12.50000000000000000 ) ) ;
#19065 = CARTESIAN_POINT ( 'NONE',  ( -8.680847955711007202, -5.923547351154968927E-13, 11.63316557810919072 ) ) ;
#19066 = CARTESIAN_POINT ( 'NONE',  ( 62.94340820527399671, 6.123233995736675563E-16, -5.000000000000007994 ) ) ;
#19067 = DIRECTION ( 'NONE',  ( 0.000000000000000000, -0.000000000000000000, -1.000000000000000000 ) ) ;
#19068 = ORIENTED_EDGE ( 'NONE', *, *, #9904, .T. ) ;
#19069 = ITEM_DEFINED_TRANSFORMATION ( 'NONE', 'NONE', #4149,  #17768 ) ;
#19070 = ORIENTED_EDGE ( 'NONE', *, *, #5493, .T. ) ;
#19071 = CARTESIAN_POINT ( 'NONE',  ( -2.000000000000000000, 2.449293598294706414E-16, 0.4999999999999995559 ) ) ;
#19072 = VECTOR ( 'NONE', #2287, 1000.000000000000000 ) ;
#19073 = CARTESIAN_POINT ( 'NONE',  ( 9.500000000000000000, 6.470877716354879437E-13, -11.20674201446023410 ) ) ;
#19074 = ORIENTED_EDGE ( 'NONE', *, *, #23165, .F. ) ;
#19075 = AXIS2_PLACEMENT_3D ( 'NONE', #19299, #4180, #13434 ) ;
#19076 = ADVANCED_FACE ( 'NONE', ( #15845 ), #14013, .F. ) ;
#19077 = CARTESIAN_POINT ( 'NONE',  ( -39.99999999999999289, 27.79189783386526358, 27.00000000000000000 ) ) ;
#19078 = ORIENTED_EDGE ( 'NONE', *, *, #19468, .T. ) ;
#19079 = CARTESIAN_POINT ( 'NONE',  ( -1.749335460928132413, -9.337549220493531976, -3.500000000000076383 ) ) ;
#19080 = VERTEX_POINT ( 'NONE', #1095 ) ;
#19081 = CARTESIAN_POINT ( 'NONE',  ( 61.48886275072855057, 7.562528597612068045E-15, 0.000000000000000000 ) ) ;
#19082 = DIRECTION ( 'NONE',  ( -0.000000000000000000, -0.000000000000000000, -1.000000000000000000 ) ) ;
#19083 = DIRECTION ( 'NONE',  ( -0.000000000000000000, -0.000000000000000000, -1.000000000000000000 ) ) ;
#19084 = CARTESIAN_POINT ( 'NONE',  ( -14.51962751333974211, 3.765689428759028790, -8.721787840009202597 ) ) ;
#19085 = VERTEX_POINT ( 'NONE', #836 ) ;
#19086 = CARTESIAN_POINT ( 'NONE',  ( 23.84999999999999432, -15.03999999999999559, 25.00000000000000000 ) ) ;
#19087 = DIRECTION ( 'NONE',  ( 0.000000000000000000, -1.000000000000000000, 0.000000000000000000 ) ) ;
#19088 = EDGE_LOOP ( 'NONE', ( #16114, #1557, #7575, #21596, #15578 ) ) ;
#19089 = CIRCLE ( 'NONE', #4291, 8.000000000000007105 ) ;
#19090 = VERTEX_POINT ( 'NONE', #12295 ) ;
#19091 = CARTESIAN_POINT ( 'NONE',  ( -9.500000000000211386, 3.086737114211961064, 10.95958914175814414 ) ) ;
#19092 = EDGE_LOOP ( 'NONE', ( #645, #3353, #4998, #21388, #1077, #22519 ) ) ;
#19093 = AXIS2_PLACEMENT_3D ( 'NONE', #15878, #14279, #8428 ) ;
#19094 = ORIENTED_EDGE ( 'NONE', *, *, #21940, .F. ) ;
#19095 = EDGE_CURVE ( 'NONE', #8837, #4471, #21514, .T. ) ;
#19096 = CARTESIAN_POINT ( 'NONE',  ( 0.000000000000000000, 0.000000000000000000, 11.99999999999999645 ) ) ;
#19097 = VERTEX_POINT ( 'NONE', #21460 ) ;
#19098 = VERTEX_POINT ( 'NONE', #2784 ) ;
#19099 = EDGE_CURVE ( 'NONE', #18612, #23407, #9785, .T. ) ;
#19100 = CARTESIAN_POINT ( 'NONE',  ( 40.23082370883257397, -29.49999999999999645, -1.500000000000000000 ) ) ;
#19101 = CARTESIAN_POINT ( 'NONE',  ( 7.022953521755574080, -5.102474405759714671, -6.433165578109188765 ) ) ;
#19102 = EDGE_CURVE ( 'NONE', #4529, #16505, #21080, .T. ) ;
#19103 = ORIENTED_EDGE ( 'NONE', *, *, #7733, .T. ) ;
#19104 = DIRECTION ( 'NONE',  ( 0.000000000000000000, 0.000000000000000000, 1.000000000000000000 ) ) ;
#19105 = DIRECTION ( 'NONE',  ( -1.000000000000000000, -0.000000000000000000, -0.000000000000000000 ) ) ;
#19106 = LINE ( 'NONE', #15542, #17995 ) ;
#19107 = DIRECTION ( 'NONE',  ( 0.000000000000000000, 0.000000000000000000, 1.000000000000000000 ) ) ;
#19108 = DIRECTION ( 'NONE',  ( 1.000000000000000000, 0.000000000000000000, 0.000000000000000000 ) ) ;
#19109 = ORIENTED_EDGE ( 'NONE', *, *, #22907, .F. ) ;
#19110 = FACE_OUTER_BOUND ( 'NONE', #6724, .T. ) ;
#19111 = CARTESIAN_POINT ( 'NONE',  ( -9.499999999999799272, -3.086737114213243593, -6.306742014460231083 ) ) ;
#19112 = AXIS2_PLACEMENT_3D ( 'NONE', #15382, #6240, #19545 ) ;
#19113 = ORIENTED_EDGE ( 'NONE', *, *, #8410, .F. ) ;
#19114 = DIRECTION ( 'NONE',  ( -0.000000000000000000, -0.000000000000000000, 1.000000000000000000 ) ) ;
#19115 = DIRECTION ( 'NONE',  ( -0.000000000000000000, -0.000000000000000000, -1.000000000000000000 ) ) ;
#19116 = CARTESIAN_POINT ( 'NONE',  ( 5.871322893124551356, -8.081182679343980269, -5.759589141758143960 ) ) ;
#19117 = CARTESIAN_POINT ( 'NONE',  ( -7.022953521754877748, -5.102474405760673015, -9.833165578109188232 ) ) ;
#19118 = CARTESIAN_POINT ( 'NONE',  ( 9.500000000000209610, -3.086737114211962396, 9.106742014460232681 ) ) ;
#19119 = ORIENTED_EDGE ( 'NONE', *, *, #1313, .F. ) ;
#19120 = VERTEX_POINT ( 'NONE', #21344 ) ;
#19121 = CARTESIAN_POINT ( 'NONE',  ( -2.682529543899159208, -8.255977015246598327, 10.03316557810918930 ) ) ;
#19122 = VERTEX_POINT ( 'NONE', #17921 ) ;
#19123 = CARTESIAN_POINT ( 'NONE',  ( 42.00000000000000000, 0.000000000000000000, 0.000000000000000000 ) ) ;
#19124 = ORIENTED_EDGE ( 'NONE', *, *, #22971, .T. ) ;
#19125 = ADVANCED_FACE ( 'NONE', ( #17668 ), #4752, .T. ) ;
#19126 = DIRECTION ( 'NONE',  ( -0.000000000000000000, -0.000000000000000000, -1.000000000000000000 ) ) ;
#19127 = PRODUCT_DEFINITION_CONTEXT ( 'detailed design', #13193, 'design' ) ;
#19128 = ADVANCED_FACE ( 'NONE', ( #10205 ), #19393, .T. ) ;
#19129 = CARTESIAN_POINT ( 'NONE',  ( 4.159489978096769569, -7.970633069177189611, 12.50000000000000000 ) ) ;
#19130 = CYLINDRICAL_SURFACE ( 'NONE', #24047, 1.000000000000000000 ) ;
#19131 = CARTESIAN_POINT ( 'NONE',  ( 79.23840997654417606, 7.420530141404717394E-15, 0.000000000000000000 ) ) ;
#19132 = ORIENTED_EDGE ( 'NONE', *, *, #21971, .F. ) ;
#19133 = DIRECTION ( 'NONE',  ( 0.000000000000000000, 0.000000000000000000, -1.000000000000000000 ) ) ;
#19134 = CARTESIAN_POINT ( 'NONE',  ( 81.85249911436491743, 6.123233995736675563E-16, -5.000000000000007994 ) ) ;
#19135 = CYLINDRICAL_SURFACE ( 'NONE', #6449, 17.87500000001787726 ) ;
#19136 = CARTESIAN_POINT ( 'NONE',  ( -41.00000000000000000, -4.000000000000000888, 9.500000000000000000 ) ) ;
#19137 = FACE_OUTER_BOUND ( 'NONE', #19677, .T. ) ;
#19138 = DIRECTION ( 'NONE',  ( 1.000000000000000000, 0.000000000000000000, 0.000000000000000000 ) ) ;
#19139 = AXIS2_PLACEMENT_3D ( 'NONE', #12678, #7189, #14634 ) ;
#19140 = CARTESIAN_POINT ( 'NONE',  ( 23.00000000000000000, -11.55437235128774809, 1.752358929577604085 ) ) ;
#19141 = ORIENTED_EDGE ( 'NONE', *, *, #3175, .T. ) ;
#19142 = CARTESIAN_POINT ( 'NONE',  ( 7.022953521754877748, 5.102474405760673903, -6.833165578109188232 ) ) ;
#19143 = AXIS2_PLACEMENT_3D ( 'NONE', #1678, #3392, #22071 ) ;
#19144 = EDGE_CURVE ( 'NONE', #18828, #11172, #19942, .T. ) ;
#19145 = EDGE_LOOP ( 'NONE', ( #4218, #10805, #2816, #16724, #17781, #18475, #15528, #17020 ) ) ;
#19146 = CARTESIAN_POINT ( 'NONE',  ( -5.871322893124554021, 8.081182679343978492, 10.75958914175814130 ) ) ;
#19147 = FACE_OUTER_BOUND ( 'NONE', #8310, .T. ) ;
#19148 = ORIENTED_EDGE ( 'NONE', *, *, #21599, .T. ) ;
#19149 = EDGE_CURVE ( 'NONE', #10247, #14507, #11792, .T. ) ;
#19150 = CARTESIAN_POINT ( 'NONE',  ( -1.029124893018731811E-15, 45.00000000000000000, 1.201721238055119212 ) ) ;
#19151 = CARTESIAN_POINT ( 'NONE',  ( 61.48886275072855057, -1.232595164407830946E-29, 5.000000000000007994 ) ) ;
#19152 = CARTESIAN_POINT ( 'NONE',  ( 41.99999999999999289, 5.618459588085056979E-15, 0.000000000000000000 ) ) ;
#19153 = VERTEX_POINT ( 'NONE', #21932 ) ;
#19154 = EDGE_CURVE ( 'NONE', #3126, #11854, #1677, .T. ) ;
#19155 = CARTESIAN_POINT ( 'NONE',  ( 2.935661446561383503, 9.035036904804158553, 6.459589141758144137 ) ) ;
#19156 = EDGE_CURVE ( 'NONE', #4737, #21717, #1459, .T. ) ;
#19157 = AXIS2_PLACEMENT_3D ( 'NONE', #4659, #17561, #15741 ) ;
#19158 = LINE ( 'NONE', #8151, #1311 ) ;
#19159 = FACE_OUTER_BOUND ( 'NONE', #17059, .T. ) ;
#19160 = CIRCLE ( 'NONE', #14851, 4.172000000000008590 ) ;
#19161 = CIRCLE ( 'NONE', #8627, 11.23082370883260772 ) ;
#19162 = ORIENTED_EDGE ( 'NONE', *, *, #370, .F. ) ;
#19163 = CYLINDRICAL_SURFACE ( 'NONE', #5957, 8.000000000000003553 ) ;
#19164 = ORIENTED_EDGE ( 'NONE', *, *, #8247, .T. ) ;
#19165 = LINE ( 'NONE', #13429, #12214 ) ;
#19166 = DIRECTION ( 'NONE',  ( 0.000000000000000000, -1.000000000000000000, 0.000000000000000000 ) ) ;
#19167 = CARTESIAN_POINT ( 'NONE',  ( 0.000000000000000000, -15.23000000000000220, 27.00000000000000000 ) ) ;
#19168 = CARTESIAN_POINT ( 'NONE',  ( 65.85249911436491743, 7.562528597612068045E-15, 0.000000000000000000 ) ) ;
#19169 = DIRECTION ( 'NONE',  ( -1.000000000000000000, 0.000000000000000000, 0.000000000000000000 ) ) ;
#19170 = FACE_OUTER_BOUND ( 'NONE', #14609, .T. ) ;
#19171 = EDGE_CURVE ( 'NONE', #17527, #2222, #12410, .T. ) ;
#19172 = CARTESIAN_POINT ( 'NONE',  ( -40.23082370883257397, -29.50000000000000711, -3.000000000000000000 ) ) ;
#19173 = AXIS2_PLACEMENT_3D ( 'NONE', #11183, #7656, #13265 ) ;
#19174 = VERTEX_POINT ( 'NONE', #19984 ) ;
#19175 = AXIS2_PLACEMENT_3D ( 'NONE', #15598, #6349, #11689 ) ;
#19176 = LINE ( 'NONE', #516, #28 ) ;
#19177 = CARTESIAN_POINT ( 'NONE',  ( -5.365059087798940141, -7.384370330707086261, 9.933165578109189653 ) ) ;
#19178 = VECTOR ( 'NONE', #11692, 1000.000000000000000 ) ;
#19179 = AXIS2_PLACEMENT_3D ( 'NONE', #19569, #6393, #10140 ) ;
#19180 = DIRECTION ( 'NONE',  ( -1.000000000000000000, -1.224606353822377258E-16, -0.000000000000000000 ) ) ;
#19181 = AXIS2_PLACEMENT_3D ( 'NONE', #7466, #14698, #20560 ) ;
#19182 = EDGE_CURVE ( 'NONE', #9192, #14126, #21815, .T. ) ;
#19183 = CARTESIAN_POINT ( 'NONE',  ( 66.72727272727273373, 4.172000000000015696, 5.109226446042767468E-16 ) ) ;
#19184 = EDGE_CURVE ( 'NONE', #12205, #8729, #14465, .T. ) ;
#19185 = EDGE_CURVE ( 'NONE', #17955, #1921, #2820, .T. ) ;
#19186 = ORIENTED_EDGE ( 'NONE', *, *, #789, .T. ) ;
#19187 = EDGE_LOOP ( 'NONE', ( #423, #20958, #17734, #17704 ) ) ;
#19188 = DIRECTION ( 'NONE',  ( -1.000000000000000000, -1.224606353822377258E-16, -0.000000000000000000 ) ) ;
#19189 = FACE_OUTER_BOUND ( 'NONE', #10699, .T. ) ;
#19190 = VERTEX_POINT ( 'NONE', #12647 ) ;
#19191 = AXIS2_PLACEMENT_3D ( 'NONE', #15761, #21383, #12340 ) ;
#19192 = AXIS2_PLACEMENT_3D ( 'NONE', #6583, #8620, #3042 ) ;
#19193 = AXIS2_PLACEMENT_3D ( 'NONE', #5019, #18061, #1358 ) ;
#19194 = ORIENTED_EDGE ( 'NONE', *, *, #3350, .F. ) ;
#19195 = LINE ( 'NONE', #664, #23320 ) ;
#19196 = AXIS2_PLACEMENT_3D ( 'NONE', #5764, #3557, #3454 ) ;
#19197 = AXIS2_PLACEMENT_3D ( 'NONE', #14076, #8692, #5056 ) ;
#19198 = ORIENTED_EDGE ( 'NONE', *, *, #4677, .T. ) ;
#19199 = CARTESIAN_POINT ( 'NONE',  ( 23.00000000000000000, 17.26667456984545623, -4.623588898214384457 ) ) ;
#19200 = AXIS2_PLACEMENT_3D ( 'NONE', #15657, #23130, #6413 ) ;
#19201 = DIRECTION ( 'NONE',  ( 0.000000000000000000, -0.000000000000000000, -1.000000000000000000 ) ) ;
#19202 = CYLINDRICAL_SURFACE ( 'NONE', #5595, 17.87500000001787726 ) ;
#19203 = PRODUCT_DEFINITION_CONTEXT ( 'detailed design', #18065, 'design' ) ;
#19204 = LINE ( 'NONE', #15641, #18504 ) ;
#19205 = VERTEX_POINT ( 'NONE', #18385 ) ;
#19206 = CARTESIAN_POINT ( 'NONE',  ( 5.000000000000000000, 4.969004387540385421E-16, -4.057500000000000107 ) ) ;
#19207 = DIRECTION ( 'NONE',  ( 1.000000000000000000, 0.000000000000000000, 0.000000000000000000 ) ) ;
#19208 = FACE_OUTER_BOUND ( 'NONE', #1546, .T. ) ;
#19209 = VERTEX_POINT ( 'NONE', #18516 ) ;
#19210 = VERTEX_POINT ( 'NONE', #16309 ) ;
#19211 = CARTESIAN_POINT ( 'NONE',  ( 2.935661446561383503, 9.035036904804158553, 4.459589141758144137 ) ) ;
#19212 = ORIENTED_EDGE ( 'NONE', *, *, #8474, .F. ) ;
#19213 = CIRCLE ( 'NONE', #8680, 17.87500000001787726 ) ;
#19214 = EDGE_CURVE ( 'NONE', #4194, #11891, #1261, .T. ) ;
#19215 = AXIS2_PLACEMENT_3D ( 'NONE', #10995, #16861, #179 ) ;
#19216 = AXIS2_PLACEMENT_3D ( 'NONE', #1303, #16527, #23981 ) ;
#19217 = EDGE_CURVE ( 'NONE', #910, #17727, #2025, .T. ) ;
#19218 = AXIS2_PLACEMENT_3D ( 'NONE', #21791, #1428, #23277 ) ;
#19219 = ORIENTED_EDGE ( 'NONE', *, *, #9747, .T. ) ;
#19220 = EDGE_LOOP ( 'NONE', ( #8211, #7814, #11335, #3929, #3593, #12109 ) ) ;
#19221 = PRODUCT_DEFINITION_SHAPE ( 'NONE', 'NONE',  #24125 ) ;
#19222 = ORIENTED_EDGE ( 'NONE', *, *, #12029, .T. ) ;
#19223 = CARTESIAN_POINT ( 'NONE',  ( 0.000000000000000000, 3.378881074890460745, -11.18737882312118082 ) ) ;
#19224 = CARTESIAN_POINT ( 'NONE',  ( -7.022953521755574080, 5.102474405759713783, -5.433165578109188765 ) ) ;
#19225 = DIRECTION ( 'NONE',  ( 0.9945797436152715720, 0.1039766011667100365, -0.000000000000000000 ) ) ;
#19226 = ORIENTED_EDGE ( 'NONE', *, *, #10561, .T. ) ;
#19227 = DIRECTION ( 'NONE',  ( -1.000000000000000000, 0.000000000000000000, 0.000000000000000000 ) ) ;
#19228 = CARTESIAN_POINT ( 'NONE',  ( 2.024999999999999911, -45.00000000000000000, -3.000000000000000000 ) ) ;
#19229 = DIRECTION ( 'NONE',  ( 0.000000000000000000, -1.000000000000000000, 0.000000000000000000 ) ) ;
#19230 = CARTESIAN_POINT ( 'NONE',  ( 0.000000000000000000, 0.000000000000000000, 0.9999999999999731326 ) ) ;
#19231 = ORIENTED_EDGE ( 'NONE', *, *, #16586, .T. ) ;
#19232 = DIRECTION ( 'NONE',  ( 0.000000000000000000, 1.000000000000000000, 0.000000000000000000 ) ) ;
#19233 = CARTESIAN_POINT ( 'NONE',  ( 5.000000000000000000, -2.342598717236905603, 4.057500000000010765 ) ) ;
#19234 = VECTOR ( 'NONE', #2945, 1000.000000000000000 ) ;
#19235 = EDGE_CURVE ( 'NONE', #12170, #23563, #3390, .T. ) ;
#19236 = ORIENTED_EDGE ( 'NONE', *, *, #10735, .F. ) ;
#19237 = CYLINDRICAL_SURFACE ( 'NONE', #1558, 40.00000000000000000 ) ;
#19238 = AXIS2_PLACEMENT_3D ( 'NONE', #15269, #6025, #4205 ) ;
#19239 = AXIS2_PLACEMENT_3D ( 'NONE', #5792, #11136, #1893 ) ;
#19240 = AXIS2_PLACEMENT_3D ( 'NONE', #2745, #925, #4709 ) ;
#19241 = CONICAL_SURFACE ( 'NONE', #7142, 4.172000000000008590, 0.9599310885968742602 ) ;
#19242 = CARTESIAN_POINT ( 'NONE',  ( 0.000000000000000000, 15.03999999999999915, -25.00000000000000000 ) ) ;
#19243 = ADVANCED_FACE ( 'NONE', ( #14724 ), #1562, .T. ) ;
#19244 = VECTOR ( 'NONE', #17116, 1000.000000000000000 ) ;
#19245 = CARTESIAN_POINT ( 'NONE',  ( -8.680847955711007202, -5.923547351154968927E-13, -5.633165578109188942 ) ) ;
#19246 = VECTOR ( 'NONE', #21452, 1000.000000000000000 ) ;
#19247 = SHAPE_REPRESENTATION ( 'End Plate', ( #8005 ), #9178 ) ;
#19248 = ORIENTED_EDGE ( 'NONE', *, *, #15292, .T. ) ;
#19249 = VERTEX_POINT ( 'NONE', #23878 ) ;
#19250 = EDGE_CURVE ( 'NONE', #4159, #3260, #486, .T. ) ;
#19251 = CARTESIAN_POINT ( 'NONE',  ( 8.680847955711007202, 5.912916378492122225E-13, 10.63316557810918894 ) ) ;
#19252 = VERTEX_POINT ( 'NONE', #4997 ) ;
#19253 =( LENGTH_UNIT ( ) NAMED_UNIT ( * ) SI_UNIT ( .MILLI., .METRE. ) );
#19254 = CARTESIAN_POINT ( 'NONE',  ( 41.99999999999999289, 25.93535998569253920, 27.00000000000000000 ) ) ;
#19255 = DIRECTION ( 'NONE',  ( -1.000000000000000000, 0.000000000000000000, 0.000000000000000000 ) ) ;
#19256 = CARTESIAN_POINT ( 'NONE',  ( -9.499999999999790390, -3.086737114213257804, -11.15958914175814520 ) ) ;
#19257 = CIRCLE ( 'NONE', #7537, 5.000000000000007994 ) ;
#19258 = CIRCLE ( 'NONE', #16903, 5.000000000000007994 ) ;
#19259 = CARTESIAN_POINT ( 'NONE',  ( -5.871322893123449127, -8.081182679344781405, -10.50674201446023304 ) ) ;
#19260 = FACE_OUTER_BOUND ( 'NONE', #3838, .T. ) ;
#19261 = CARTESIAN_POINT ( 'NONE',  ( -9.499999999999799272, -3.086737114213243593, 6.306742014460231083 ) ) ;
#19262 = AXIS2_PLACEMENT_3D ( 'NONE', #8079, #10286, #15524 ) ;
#19263 = AXIS2_PLACEMENT_3D ( 'NONE', #1736, #14298, #10624 ) ;
#19264 = CARTESIAN_POINT ( 'NONE',  ( -29.00000000000000000, -29.49999999999999645, 11.00000000000000000 ) ) ;
#19265 = DIRECTION ( 'NONE',  ( 1.000000000000000000, -2.600433232233976523E-16, 0.000000000000000000 ) ) ;
#19266 = VECTOR ( 'NONE', #9613, 1000.000000000000000 ) ;
#19267 = LINE ( 'NONE', #22929, #5658 ) ;
#19268 = ORIENTED_EDGE ( 'NONE', *, *, #1882, .F. ) ;
#19269 = CARTESIAN_POINT ( 'NONE',  ( 41.00000000000000000, -6.000000000000015099, 11.00000000000000000 ) ) ;
#19270 = FACE_OUTER_BOUND ( 'NONE', #3417, .T. ) ;
#19271 = DIRECTION ( 'NONE',  ( -1.000000000000000000, 0.000000000000000000, 0.000000000000000000 ) ) ;
#19272 = CARTESIAN_POINT ( 'NONE',  ( -45.00000000000000000, -50.99999999999993605, 12.50000000000000000 ) ) ;
#19273 = EDGE_CURVE ( 'NONE', #9582, #6887, #21908, .T. ) ;
#19274 = ORIENTED_EDGE ( 'NONE', *, *, #12812, .T. ) ;
#19275 = CARTESIAN_POINT ( 'NONE',  ( -5.365059087799947335, 7.384370330706355290, -5.333165578109189120 ) ) ;
#19276 = AXIS2_PLACEMENT_3D ( 'NONE', #11008, #4085, #307 ) ;
#19277 = ORIENTED_EDGE ( 'NONE', *, *, #6902, .F. ) ;
#19278 = CARTESIAN_POINT ( 'NONE',  ( 9.500000000000000000, 6.470877716354879437E-13, 12.05958914175814378 ) ) ;
#19279 = DIRECTION ( 'NONE',  ( -1.000000000000000000, -1.224606353822377258E-16, -0.000000000000000000 ) ) ;
#19280 = CIRCLE ( 'NONE', #14592, 2.024999999999999911 ) ;
#19281 = ORIENTED_EDGE ( 'NONE', *, *, #20956, .T. ) ;
#19282 =( LENGTH_UNIT ( ) NAMED_UNIT ( * ) SI_UNIT ( .MILLI., .METRE. ) );
#19283 = LINE ( 'NONE', #5979, #22378 ) ;
#19284 = CARTESIAN_POINT ( 'NONE',  ( 42.00000000000000000, 0.000000000000000000, 11.00000000000000000 ) ) ;
#19285 = DIRECTION ( 'NONE',  ( -1.000000000000000000, -0.000000000000000000, -0.000000000000000000 ) ) ;
#19286 = CARTESIAN_POINT ( 'NONE',  ( 40.89823313241238623, -26.41789760203348081, 27.00000000000000000 ) ) ;
#19287 = DIRECTION ( 'NONE',  ( -0.000000000000000000, -0.000000000000000000, -1.000000000000000000 ) ) ;
#19288 = CARTESIAN_POINT ( 'NONE',  ( 0.000000000000000000, 12.00453763395396756, -1.558955687733494244 ) ) ;
#19289 = AXIS2_PLACEMENT_3D ( 'NONE', #13957, #1035, #23365 ) ;
#19290 = DIRECTION ( 'NONE',  ( 0.7071067811865493491, 0.000000000000000000, 0.7071067811865456854 ) ) ;
#19291 = ORIENTED_EDGE ( 'NONE', *, *, #23660, .F. ) ;
#19292 = CIRCLE ( 'NONE', #21242, 11.68650000001168721 ) ;
#19293 = ORIENTED_EDGE ( 'NONE', *, *, #3538, .F. ) ;
#19294 = DIRECTION ( 'NONE',  ( -0.000000000000000000, -0.000000000000000000, 1.000000000000000000 ) ) ;
#19295 = FACE_OUTER_BOUND ( 'NONE', #4955, .T. ) ;
#19296 = CARTESIAN_POINT ( 'NONE',  ( 5.000000000000000000, 0.000000000000000000, 0.000000000000000000 ) ) ;
#19297 = DIRECTION ( 'NONE',  ( -0.5735764363510519326, 0.8191520442889876907, 1.003171929053519816E-16 ) ) ;
#19298 = ADVANCED_FACE ( 'NONE', ( #14599 ), #3144, .T. ) ;
#19299 = CARTESIAN_POINT ( 'NONE',  ( -34.00000000000000000, -3.999999999999999112, 10.49999999999999822 ) ) ;
#19300 = EDGE_CURVE ( 'NONE', #21933, #16608, #18032, .T. ) ;
#19301 = DIRECTION ( 'NONE',  ( -0.5735764363510519326, 0.8191520442889876907, 1.003171929053519816E-16 ) ) ;
#19302 = EDGE_CURVE ( 'NONE', #15047, #16347, #12512, .T. ) ;
#19303 = CARTESIAN_POINT ( 'NONE',  ( 39.99999999999999289, 27.79189783386526358, 27.00000000000000000 ) ) ;
#19304 = CARTESIAN_POINT ( 'NONE',  ( 23.00000000000000000, 14.21257171757157245, 0.08908218613057176938 ) ) ;
#19305 = VECTOR ( 'NONE', #1241, 1000.000000000000000 ) ;
#19306 = AXIS2_PLACEMENT_3D ( 'NONE', #6574, #7031, #3384 ) ;
#19307 = ORIENTED_EDGE ( 'NONE', *, *, #20420, .F. ) ;
#19308 = CARTESIAN_POINT ( 'NONE',  ( 5.871322893123449127, 8.081182679344781405, -7.506742014460233037 ) ) ;
#19309 = ORIENTED_EDGE ( 'NONE', *, *, #13151, .F. ) ;
#19310 = DIRECTION ( 'NONE',  ( -1.000000000000000000, -1.224606353822377258E-16, -0.000000000000000000 ) ) ;
#19311 = CARTESIAN_POINT ( 'NONE',  ( 2.682529543899157876, 8.255977015246598327, 7.033165578109189298 ) ) ;
#19312 = CARTESIAN_POINT ( 'NONE',  ( 0.000000000000000000, -15.03999999999999915, 25.00000000000000000 ) ) ;
#19313 = DIRECTION ( 'NONE',  ( -1.000000000000000000, 0.000000000000000000, 0.000000000000000000 ) ) ;
#19314 = CARTESIAN_POINT ( 'NONE',  ( 4.489900896931573904, 0.000000000000000000, 0.000000000000000000 ) ) ;
#19315 = APPLICATION_CONTEXT ( 'automotive_design' ) ;
#19316 = AXIS2_PLACEMENT_3D ( 'NONE', #11575, #11314, #143 ) ;
#19317 = EDGE_LOOP ( 'NONE', ( #13456, #10118, #70, #11139, #6187, #1815 ) ) ;
#19318 = ITEM_DEFINED_TRANSFORMATION ( 'NONE', 'NONE', #23994,  #8005 ) ;
#19319 = VERTEX_POINT ( 'NONE', #23663 ) ;
#19320 = DIRECTION ( 'NONE',  ( 0.000000000000000000, 0.000000000000000000, 1.000000000000000000 ) ) ;
#19321 = CIRCLE ( 'NONE', #6852, 10.50249999999999950 ) ;
#19322 = CIRCLE ( 'NONE', #2600, 19.84999999999999787 ) ;
#19323 = EDGE_CURVE ( 'NONE', #20443, #9461, #14357, .T. ) ;
#19324 = CARTESIAN_POINT ( 'NONE',  ( -9.500000000000000000, -6.482511860946779655E-13, -12.20674201446023410 ) ) ;
#19325 = VERTEX_POINT ( 'NONE', #4233 ) ;
#19326 = DIRECTION ( 'NONE',  ( -0.000000000000000000, -0.000000000000000000, 1.000000000000000000 ) ) ;
#19327 = CARTESIAN_POINT ( 'NONE',  ( 0.000000000000000000, 0.000000000000000000, 0.000000000000000000 ) ) ;
#19328 = ORIENTED_EDGE ( 'NONE', *, *, #14687, .F. ) ;
#19329 = CARTESIAN_POINT ( 'NONE',  ( 85.63636363636365445, -4.172000000000000597, 5.616230220889771312E-16 ) ) ;
#19330 = EDGE_CURVE ( 'NONE', #12646, #1909, #20586, .T. ) ;
#19331 = EDGE_CURVE ( 'NONE', #9243, #898, #11345, .T. ) ;
#19332 = ORIENTED_EDGE ( 'NONE', *, *, #9174, .F. ) ;
#19333 = EDGE_CURVE ( 'NONE', #12080, #10011, #20737, .T. ) ;
#19334 = AXIS2_PLACEMENT_3D ( 'NONE', #21391, #20042, #14405 ) ;
#19335 = DIRECTION ( 'NONE',  ( -0.000000000000000000, -0.000000000000000000, 1.000000000000000000 ) ) ;
#19336 = EDGE_CURVE ( 'NONE', #12319, #6874, #10200, .T. ) ;
#19337 = DIRECTION ( 'NONE',  ( -0.000000000000000000, 0.000000000000000000, 1.000000000000000000 ) ) ;
#19338 = LINE ( 'NONE', #22989, #19653 ) ;
#19339 =( GEOMETRIC_REPRESENTATION_CONTEXT ( 3 ) GLOBAL_UNCERTAINTY_ASSIGNED_CONTEXT ( ( #19626 ) ) GLOBAL_UNIT_ASSIGNED_CONTEXT ( ( #8270, #23319, #13781 ) ) REPRESENTATION_CONTEXT ( 'NONE', 'WORKASPACE' ) );
#19340 = AXIS2_PLACEMENT_3D ( 'NONE', #21234, #4536, #15975 ) ;
#19341 = DIRECTION ( 'NONE',  ( -0.7089874389501492624, 0.7052211081716913688, 0.000000000000000000 ) ) ;
#19342 = ORIENTED_EDGE ( 'NONE', *, *, #8742, .F. ) ;
#19343 = DIRECTION ( 'NONE',  ( 0.000000000000000000, 1.000000000000000000, 0.000000000000000000 ) ) ;
#19344 = CYLINDRICAL_SURFACE ( 'NONE', #12981, 14.99999999999999822 ) ;
#19345 = ORIENTED_EDGE ( 'NONE', *, *, #22146, .F. ) ;
#19346 = CIRCLE ( 'NONE', #15414, 1.499999999999994449 ) ;
#19347 = VECTOR ( 'NONE', #3080, 1000.000000000000000 ) ;
#19348 = ORIENTED_EDGE ( 'NONE', *, *, #17397, .T. ) ;
#19349 = CARTESIAN_POINT ( 'NONE',  ( 9.500000000000000000, 6.470877716354879437E-13, 6.059589141758143782 ) ) ;
#19350 = EDGE_LOOP ( 'NONE', ( #6161, #7250, #22545, #7888 ) ) ;
#19351 = EDGE_LOOP ( 'NONE', ( #19309, #18620, #20915 ) ) ;
#19352 = ORIENTED_EDGE ( 'NONE', *, *, #16258, .T. ) ;
#19353 = ORIENTED_EDGE ( 'NONE', *, *, #11055, .F. ) ;
#19354 = CARTESIAN_POINT ( 'NONE',  ( 23.97500000000000497, -29.50000000000000000, -3.000000000000000000 ) ) ;
#19355 = CARTESIAN_POINT ( 'NONE',  ( 5.365059087798938364, 7.384370330707087149, -6.933165578109188765 ) ) ;
#19356 = AXIS2_PLACEMENT_3D ( 'NONE', #18378, #23527, #16544 ) ;
#19357 = PRODUCT_DEFINITION_FORMATION_WITH_SPECIFIED_SOURCE ( 'ANY', '', #1973, .NOT_KNOWN. ) ;
#19358 = ADVANCED_FACE ( 'NONE', ( #11268 ), #7390, .T. ) ;
#19359 = CIRCLE ( 'NONE', #10372, 11.68650000001168543 ) ;
#19360 = EDGE_LOOP ( 'NONE', ( #12738, #16609, #16807 ) ) ;
#19361 = CARTESIAN_POINT ( 'NONE',  ( -20.85000000000000497, 15.03999999999999915, 0.000000000000000000 ) ) ;
#19362 = DIRECTION ( 'NONE',  ( 1.000000000000000000, 0.000000000000000000, 0.000000000000000000 ) ) ;
#19363 = DIRECTION ( 'NONE',  ( -1.000000000000000000, 0.000000000000000000, 0.000000000000000000 ) ) ;
#19364 = ORIENTED_EDGE ( 'NONE', *, *, #2343, .F. ) ;
#19365 = CIRCLE ( 'NONE', #15835, 1.999999999999996669 ) ;
#19367 = ADVANCED_FACE ( 'NONE', ( #22425 ), #5151, .T. ) ;
#19366 = LINE ( 'NONE', #21673, #20775 ) ;
#19368 = ORIENTED_EDGE ( 'NONE', *, *, #9628, .F. ) ;
#19369 = DIRECTION ( 'NONE',  ( 1.000000000000000000, 0.000000000000000000, 0.000000000000000000 ) ) ;
#19370 = ADVANCED_FACE ( 'NONE', ( #14827 ), #18633, .T. ) ;
#19371 = FILL_AREA_STYLE ('',( #445 ) ) ;
#19372 = CARTESIAN_POINT ( 'NONE',  ( 16.68617496892349905, -7.233372502334337817, 6.175747996014750996 ) ) ;
#19373 = DIRECTION ( 'NONE',  ( -1.000000000000000000, 0.000000000000000000, 0.000000000000000000 ) ) ;
#19374 = CARTESIAN_POINT ( 'NONE',  ( 6.222797240145152671E-13, -9.127583699786111282, -8.133165578109188942 ) ) ;
#19375 = AXIS2_PLACEMENT_3D ( 'NONE', #14900, #22719, #22372 ) ;
#19376 = DIRECTION ( 'NONE',  ( 1.000000000000000000, -6.938893903907222067E-15, 0.000000000000000000 ) ) ;
#19377 = ORIENTED_EDGE ( 'NONE', *, *, #10211, .F. ) ;
#19378 = VERTEX_POINT ( 'NONE', #16907 ) ;
#19379 = VERTEX_POINT ( 'NONE', #13502 ) ;
#19380 = CARTESIAN_POINT ( 'NONE',  ( 0.000000000000000000, 0.000000000000000000, 0.000000000000000000 ) ) ;
#19381 = DIRECTION ( 'NONE',  ( 0.000000000000000000, 0.000000000000000000, 1.000000000000000000 ) ) ;
#19382 = ORIENTED_EDGE ( 'NONE', *, *, #9879, .F. ) ;
#19383 = DIRECTION ( 'NONE',  ( -1.000000000000000000, 0.000000000000000000, 0.000000000000000000 ) ) ;
#19384 = DIRECTION ( 'NONE',  ( -1.000000000000000000, 0.000000000000000000, 0.000000000000000000 ) ) ;
#19385 = CARTESIAN_POINT ( 'NONE',  ( 6.809999908187194197E-13, -9.988891130263535700, -10.70674201446023410 ) ) ;
#19386 = DIRECTION ( 'NONE',  ( 1.000000000000000000, 0.000000000000000000, 0.000000000000000000 ) ) ;
#19387 = DIRECTION ( 'NONE',  ( 0.000000000000000000, -1.000000000000000000, 0.000000000000000000 ) ) ;
#19388 = EDGE_CURVE ( 'NONE', #17416, #2169, #97, .T. ) ;
#19389 = ORIENTED_EDGE ( 'NONE', *, *, #9756, .T. ) ;
#19390 = FACE_OUTER_BOUND ( 'NONE', #8829, .T. ) ;
#19391 = LINE ( 'NONE', #6313, #1277 ) ;
#19392 = CARTESIAN_POINT ( 'NONE',  ( 0.000000000000000000, 45.00000000000000000, -23.99999999999999645 ) ) ;
#19393 = CYLINDRICAL_SURFACE ( 'NONE', #8231, 5.000000000000000888 ) ;
#19394 = EDGE_CURVE ( 'NONE', #21975, #20352, #21533, .T. ) ;
#19395 = CARTESIAN_POINT ( 'NONE',  ( 0.000000000000000000, -45.00000000000000000, -27.00000000000000000 ) ) ;
#19396 = DIRECTION ( 'NONE',  ( -0.000000000000000000, -0.000000000000000000, -1.000000000000000000 ) ) ;
#19397 = CARTESIAN_POINT ( 'NONE',  ( 0.000000000000000000, -45.00000000000000000, 27.00000000000000000 ) ) ;
#19398 = ORIENTED_EDGE ( 'NONE', *, *, #23341, .F. ) ;
#19399 = CARTESIAN_POINT ( 'NONE',  ( -5.871322893123450015, -8.081182679344781405, -12.50674201446023481 ) ) ;
#19400 = ORIENTED_EDGE ( 'NONE', *, *, #14188, .F. ) ;
#19401 = ORIENTED_EDGE ( 'NONE', *, *, #4266, .F. ) ;
#19402 = CARTESIAN_POINT ( 'NONE',  ( -7.685661446561619314, -5.583959896779019161, 9.259589141758143072 ) ) ;
#19403 = CARTESIAN_POINT ( 'NONE',  ( 7.685661446562381371, -5.583959896777971110, 13.00674201446023304 ) ) ;
#19404 = VERTEX_POINT ( 'NONE', #7628 ) ;
#19405 = CARTESIAN_POINT ( 'NONE',  ( -7.022953521754877748, -5.102474405760673015, -11.83316557810918823 ) ) ;
#19406 = FACE_OUTER_BOUND ( 'NONE', #15157, .T. ) ;
#19407 = DIRECTION ( 'NONE',  ( -0.000000000000000000, -0.000000000000000000, -1.000000000000000000 ) ) ;
#19408 = CARTESIAN_POINT ( 'NONE',  ( 61.78386452199871570, 7.420530141404717394E-15, 0.000000000000000000 ) ) ;
#19409 = EDGE_CURVE ( 'NONE', #13080, #17379, #21119, .T. ) ;
#19410 = CARTESIAN_POINT ( 'NONE',  ( 15.00000000000000355, -0.3238088414458117903, -9.499999999999987566 ) ) ;
#19411 = DIRECTION ( 'NONE',  ( 0.000000000000000000, 0.5406408174555987767, -0.8412535328311804284 ) ) ;
#19412 = CARTESIAN_POINT ( 'NONE',  ( 82.72727272727273373, 7.491529369508391930E-15, 0.000000000000000000 ) ) ;
#19413 = EDGE_CURVE ( 'NONE', #9925, #8713, #9039, .T. ) ;
#19415 = EDGE_CURVE ( 'NONE', #1909, #17518, #16814, .T. ) ;
#19414 = FACE_BOUND ( 'NONE', #18400, .T. ) ;
#19416 = EDGE_LOOP ( 'NONE', ( #4498, #23229, #10938 ) ) ;
#19417 = ORIENTED_EDGE ( 'NONE', *, *, #7026, .F. ) ;
#19418 = FACE_OUTER_BOUND ( 'NONE', #13526, .T. ) ;
#19419 = CARTESIAN_POINT ( 'NONE',  ( -8.818858540945930358, -3.028632380371159449, 12.18357898287954733 ) ) ;
#19420 = VECTOR ( 'NONE', #20455, 1000.000000000000000 ) ;
#19421 = CARTESIAN_POINT ( 'NONE',  ( -2.935661446561384391, -9.035036904804158553, 11.45958914175814414 ) ) ;
#19422 = CARTESIAN_POINT ( 'NONE',  ( 40.23082370883257397, -27.62204025492844650, -3.000000000000000000 ) ) ;
#19423 = CARTESIAN_POINT ( 'NONE',  ( 23.00000000000000000, -8.772759796005278332, 7.720943453482002283 ) ) ;
#19424 = ORIENTED_EDGE ( 'NONE', *, *, #13219, .T. ) ;
#19425 = CARTESIAN_POINT ( 'NONE',  ( -41.73082370883260239, 50.99999999999999289, 0.000000000000000000 ) ) ;
#19426 = LINE ( 'NONE', #21116, #23214 ) ;
#19427 = VERTEX_POINT ( 'NONE', #92 ) ;
#19428 = CARTESIAN_POINT ( 'NONE',  ( -9.500000000000000000, -6.482511860946779655E-13, -8.206742014460234103 ) ) ;
#19429 = VERTEX_POINT ( 'NONE', #7745 ) ;
#19430 = CARTESIAN_POINT ( 'NONE',  ( 29.00000000000000000, 29.50000000000000000, 14.00000000000000178 ) ) ;
#19431 = CARTESIAN_POINT ( 'NONE',  ( 6.222797240145152671E-13, -9.127583699786111282, 10.13316557810918894 ) ) ;
#19432 = DIRECTION ( 'NONE',  ( 0.000000000000000000, -1.000000000000000000, 0.000000000000000000 ) ) ;
#19433 = FACE_OUTER_BOUND ( 'NONE', #7239, .T. ) ;
#19434 = DIRECTION ( 'NONE',  ( 1.000000000000000000, 1.224606353822377258E-16, 0.000000000000000000 ) ) ;
#19435 = CIRCLE ( 'NONE', #10453, 2.500000000000002220 ) ;
#19436 = VERTEX_POINT ( 'NONE', #15177 ) ;
#19437 = EDGE_CURVE ( 'NONE', #11621, #9659, #3629, .T. ) ;
#19438 = ORIENTED_EDGE ( 'NONE', *, *, #14103, .T. ) ;
#19439 = DIRECTION ( 'NONE',  ( 1.000000000000000000, 0.000000000000000000, 0.000000000000000000 ) ) ;
#19440 = EDGE_CURVE ( 'NONE', #13688, #22991, #12153, .T. ) ;
#19441 = CARTESIAN_POINT ( 'NONE',  ( 23.00000000000000000, 12.02595010061972403, -13.22467954916275268 ) ) ;
#19442 = ORIENTED_EDGE ( 'NONE', *, *, #4991, .F. ) ;
#19443 = CARTESIAN_POINT ( 'NONE',  ( 3.934052222107162766, -8.094642247421043990, -12.50000000000000000 ) ) ;
#19444 = DIRECTION ( 'NONE',  ( 0.000000000000000000, 0.000000000000000000, 1.000000000000000000 ) ) ;
#19445 = ORIENTED_EDGE ( 'NONE', *, *, #12348, .F. ) ;
#19446 = CARTESIAN_POINT ( 'NONE',  ( -40.23082370883257397, -29.50000000000000711, -3.000000000000000000 ) ) ;
#19447 = ORIENTED_EDGE ( 'NONE', *, *, #5870, .T. ) ;
#19448 = CARTESIAN_POINT ( 'NONE',  ( 90.00000000000000000, 4.171999999999999709, 0.000000000000000000 ) ) ;
#19449 = FACE_OUTER_BOUND ( 'NONE', #20209, .T. ) ;
#19450 = FACE_OUTER_BOUND ( 'NONE', #9310, .T. ) ;
#19451 = CARTESIAN_POINT ( 'NONE',  ( -40.23082370883260239, 27.62204025492846071, -3.000000000000000000 ) ) ;
#19452 = VERTEX_POINT ( 'NONE', #4113 ) ;
#19453 = CARTESIAN_POINT ( 'NONE',  ( -44.00000000000000711, -51.00000000000000711, 0.5000000000000000000 ) ) ;
#19454 = CARTESIAN_POINT ( 'NONE',  ( -45.00000000000001421, 50.99999999999992184, 12.50000000000000000 ) ) ;
#19455 = CARTESIAN_POINT ( 'NONE',  ( 9.500000000000000000, 6.470877716354879437E-13, 9.206742014460234103 ) ) ;
#19456 = EDGE_LOOP ( 'NONE', ( #18643, #18395, #16274, #9004 ) ) ;
#19457 = ORIENTED_EDGE ( 'NONE', *, *, #18961, .T. ) ;
#19458 = CARTESIAN_POINT ( 'NONE',  ( -7.685661446562381371, 5.583959896777970222, 6.859589141758143604 ) ) ;
#19459 = EDGE_CURVE ( 'NONE', #1636, #19800, #17917, .T. ) ;
#19460 = ORIENTED_EDGE ( 'NONE', *, *, #9608, .T. ) ;
#19461 = ORIENTED_EDGE ( 'NONE', *, *, #11058, .T. ) ;
#19462 = ADVANCED_FACE ( 'NONE', ( #17270 ), #6429, .T. ) ;
#19463 = ORIENTED_EDGE ( 'NONE', *, *, #24070, .T. ) ;
#19464 = EDGE_CURVE ( 'NONE', #678, #6052, #15442, .T. ) ;
#19465 = ORIENTED_EDGE ( 'NONE', *, *, #21, .T. ) ;
#19466 = DIRECTION ( 'NONE',  ( -1.000000000000000000, 0.000000000000000000, 0.000000000000000000 ) ) ;
#19467 = CARTESIAN_POINT ( 'NONE',  ( 5.365059087798938364, 7.384370330707087149, -4.933165578109187877 ) ) ;
#19468 = EDGE_CURVE ( 'NONE', #6547, #15558, #7372, .T. ) ;
#19469 = CARTESIAN_POINT ( 'NONE',  ( -14.99999999999999822, 6.045577542124163753E-21, -9.499999999999994671 ) ) ;
#19470 = DIRECTION ( 'NONE',  ( -0.9160001545545232160, 0.4011779117250717785, 0.000000000000000000 ) ) ;
#19471 = EDGE_LOOP ( 'NONE', ( #9541, #11305, #13223, #19804 ) ) ;
#19472 = CARTESIAN_POINT ( 'NONE',  ( -17.15242344757784210, -8.297343789534776803, 4.632629386303505292 ) ) ;
#19473 = DIRECTION ( 'NONE',  ( 0.000000000000000000, -1.000000000000000000, 0.000000000000000000 ) ) ;
#19474 = AXIS2_PLACEMENT_3D ( 'NONE', #15669, #11890, #17624 ) ;
#19475 = CARTESIAN_POINT ( 'NONE',  ( 1.999999999999994449, -45.00000000000000000, 3.000000000000002665 ) ) ;
#19476 = EDGE_LOOP ( 'NONE', ( #18689, #7437, #12422, #16799 ) ) ;
#19477 = DIRECTION ( 'NONE',  ( 0.7089874389501492624, 0.7052211081716913688, 0.000000000000000000 ) ) ;
#19478 = DIRECTION ( 'NONE',  ( 0.000000000000000000, -1.000000000000000000, 0.000000000000000000 ) ) ;
#19479 = ORIENTED_EDGE ( 'NONE', *, *, #3345, .F. ) ;
#19480 = CARTESIAN_POINT ( 'NONE',  ( 35.99999999999999289, 50.99999999999999289, 0.5000000000000004441 ) ) ;
#19481 = DIRECTION ( 'NONE',  ( -0.000000000000000000, -0.000000000000000000, -1.000000000000000000 ) ) ;
#19482 = AXIS2_PLACEMENT_3D ( 'NONE', #16190, #14110, #5199 ) ;
#19483 = CARTESIAN_POINT ( 'NONE',  ( 16.08510323282434484, -6.088885580147184839, -7.295537496892074536 ) ) ;
#19484 = AXIS2_PLACEMENT_3D ( 'NONE', #16283, #14438, #23745 ) ;
#19485 = DIRECTION ( 'NONE',  ( -1.000000000000000000, -1.224606353822377258E-16, -0.000000000000000000 ) ) ;
#19486 = CARTESIAN_POINT ( 'NONE',  ( 2.682529543899157876, 8.255977015246598327, -9.033165578109187521 ) ) ;
#19487 = CARTESIAN_POINT ( 'NONE',  ( 29.00000000000000711, -29.50000000000000711, 27.00000000000000000 ) ) ;
#19488 = EDGE_CURVE ( 'NONE', #5422, #732, #4684, .T. ) ;
#19489 = VERTEX_POINT ( 'NONE', #21431 ) ;
#19490 = CARTESIAN_POINT ( 'NONE',  ( -8.680847955711200825, 2.820578480813073607, 9.533165578109187521 ) ) ;
#19491 = VERTEX_POINT ( 'NONE', #4848 ) ;
#19492 = DIRECTION ( 'NONE',  ( 1.000000000000000000, 0.000000000000000000, 0.000000000000000000 ) ) ;
#19493 = DIRECTION ( 'NONE',  ( -0.000000000000000000, -0.000000000000000000, -1.000000000000000000 ) ) ;
#19494 = ORIENTED_EDGE ( 'NONE', *, *, #5386, .F. ) ;
#19495 = EDGE_CURVE ( 'NONE', #2222, #721, #2881, .T. ) ;
#19496 = FACE_OUTER_BOUND ( 'NONE', #11309, .T. ) ;
#19497 = CARTESIAN_POINT ( 'NONE',  ( -5.871322893123450015, -8.081182679344781405, -11.35958914175814272 ) ) ;
#19498 = EDGE_CURVE ( 'NONE', #5066, #9263, #10467, .T. ) ;
#19499 = AXIS2_PLACEMENT_3D ( 'NONE', #14502, #20259, #1711 ) ;
#19500 = CARTESIAN_POINT ( 'NONE',  ( 1.830024671936552272, 8.813519001246380213, 101.3851422246032570 ) ) ;
#19501 = CARTESIAN_POINT ( 'NONE',  ( 10.00000000000000178, 0.000000000000000000, 0.000000000000000000 ) ) ;
#19502 = DIRECTION ( 'NONE',  ( 0.000000000000000000, 0.000000000000000000, -1.000000000000000000 ) ) ;
#19503 = ORIENTED_EDGE ( 'NONE', *, *, #17295, .F. ) ;
#19504 = DIRECTION ( 'NONE',  ( -0.000000000000000000, 0.000000000000000000, 1.000000000000000000 ) ) ;
#19505 = CARTESIAN_POINT ( 'NONE',  ( 0.000000000000000000, -45.00000000000000000, 27.00000000000000000 ) ) ;
#19506 = CARTESIAN_POINT ( 'NONE',  ( 35.99999999999999289, 50.99999999999999289, 0.000000000000000000 ) ) ;
#19507 = DIRECTION ( 'NONE',  ( 0.000000000000000000, -0.7557495743542635980, 0.6548607339452787723 ) ) ;
#19508 = DIRECTION ( 'NONE',  ( 0.000000000000000000, -1.000000000000000000, 0.000000000000000000 ) ) ;
#19509 = CARTESIAN_POINT ( 'NONE',  ( 40.00000000000000000, -27.79189783386526358, -27.00000000000000000 ) ) ;
#19510 = DIRECTION ( 'NONE',  ( -1.000000000000000000, -1.224606353822377258E-16, -0.000000000000000000 ) ) ;
#19511 = ORIENTED_EDGE ( 'NONE', *, *, #17180, .T. ) ;
#19512 = CARTESIAN_POINT ( 'NONE',  ( 2.935661446561383503, 9.035036904804158553, -11.60674201446023268 ) ) ;
#19513 = VERTEX_POINT ( 'NONE', #1066 ) ;
#19514 = ORIENTED_EDGE ( 'NONE', *, *, #8822, .T. ) ;
#19515 = AXIS2_PLACEMENT_3D ( 'NONE', #11593, #6500, #17209 ) ;
#19516 = B_SPLINE_CURVE_WITH_KNOTS ( 'NONE', 3,
 ( #5674, #13097, #13211, #3717 ),
 .UNSPECIFIED., .F., .F.,
 ( 4, 4 ),
 ( 0.000000000000000000, 1.000000000000000000 ),
 .UNSPECIFIED. ) ;
#19517 = CARTESIAN_POINT ( 'NONE',  ( -5.871322893123450015, -8.081182679344781405, 5.359589141758144493 ) ) ;
#19518 = CARTESIAN_POINT ( 'NONE',  ( 9.500000000000000000, 6.470877716354879437E-13, 11.20674201446023410 ) ) ;
#19519 = ORIENTED_EDGE ( 'NONE', *, *, #6077, .F. ) ;
#19520 = CARTESIAN_POINT ( 'NONE',  ( 0.000000000000000000, 0.000000000000000000, 0.000000000000000000 ) ) ;
#19521 = PLANE ( 'NONE',  #7220 ) ;
#19522 = LINE ( 'NONE', #23192, #14260 ) ;
#19523 = CARTESIAN_POINT ( 'NONE',  ( 2.454813078130514813E-15, -16.67999999999999972, 13.00000000000000178 ) ) ;
#19524 = EDGE_CURVE ( 'NONE', #8401, #379, #10496, .T. ) ;
#19525 = FACE_OUTER_BOUND ( 'NONE', #14413, .T. ) ;
#19526 = CARTESIAN_POINT ( 'NONE',  ( 42.00000000000000000, 0.000000000000000000, 12.00000000000000000 ) ) ;
#19527 = DIRECTION ( 'NONE',  ( -0.5735764363510519326, 0.8191520442889876907, 1.003171929053519816E-16 ) ) ;
#19528 =( BOUNDED_CURVE ( )  B_SPLINE_CURVE ( 2, ( #13007, #1915, #9333, #16778, #20587, #93, #17031, #21059, #2520, #7746, #4234 ),
 .UNSPECIFIED., .F., .F. ) 
 B_SPLINE_CURVE_WITH_KNOTS ( ( 3, 2, 2, 2, 2, 3 ),
 ( 0.3000000000000000999, 0.3200000000000001177, 0.3400000000000000799, 0.3600000000000000422, 0.3800000000000000044, 0.4000000000000000222 ),
 .UNSPECIFIED. ) 
 CURVE ( )  GEOMETRIC_REPRESENTATION_ITEM ( )  RATIONAL_B_SPLINE_CURVE ( ( 0.9999999999999997780, 0.9510565162951537532, 1.000000000000000000, 0.9510565162951535312, 1.000000000000000000, 0.9510565162951535312, 1.000000000000000000, 0.9510565162951535312, 1.000000000000000000, 0.9510565162951535312, 1.000000000000000000 ) ) 
 REPRESENTATION_ITEM ( '' )  );
#19529 = VERTEX_POINT ( 'NONE', #570 ) ;
#19530 = AXIS2_PLACEMENT_3D ( 'NONE', #16683, #22077, #9236 ) ;
#19531 = CARTESIAN_POINT ( 'NONE',  ( 86.21613547800127719, 5.000000000000015987, 0.000000000000000000 ) ) ;
#19532 = ORIENTED_EDGE ( 'NONE', *, *, #3940, .T. ) ;
#19533 = CARTESIAN_POINT ( 'NONE',  ( 23.00000000000000000, -13.61176534793449200, 10.13961790095610560 ) ) ;
#19534 = PLANE ( 'NONE',  #20021 ) ;
#19535 = CIRCLE ( 'NONE', #14841, 1.000000000000000888 ) ;
#19536 = DIRECTION ( 'NONE',  ( -0.000000000000000000, -0.000000000000000000, -1.000000000000000000 ) ) ;
#19537 = CARTESIAN_POINT ( 'NONE',  ( 9.330908268522556170, -1.784418920662232289, 11.99999999999997691 ) ) ;
#19538 = DIRECTION ( 'NONE',  ( -1.000000000000000000, 2.600433232233976523E-16, 0.000000000000000000 ) ) ;
#19539 = EDGE_LOOP ( 'NONE', ( #10297, #8052, #6951, #1147 ) ) ;
#19540 = EDGE_CURVE ( 'NONE', #5523, #12511, #19602, .T. ) ;
#19541 = DIRECTION ( 'NONE',  ( 1.000000000000000000, 0.000000000000000000, 0.000000000000000000 ) ) ;
#19542 = ORIENTED_EDGE ( 'NONE', *, *, #6491, .F. ) ;
#19543 = DIRECTION ( 'NONE',  ( 0.000000000000000000, 0.9898214418809322401, 0.1423148382732887240 ) ) ;
#19544 = VERTEX_POINT ( 'NONE', #6180 ) ;
#19545 = DIRECTION ( 'NONE',  ( 0.000000000000000000, -1.000000000000000000, 0.000000000000000000 ) ) ;
#19546 = EDGE_CURVE ( 'NONE', #5954, #1470, #12010, .T. ) ;
#19547 = CARTESIAN_POINT ( 'NONE',  ( 2.682529543900284974, -8.255977015246234174, 4.233165578109187699 ) ) ;
#19548 = DIRECTION ( 'NONE',  ( -0.000000000000000000, -0.000000000000000000, -1.000000000000000000 ) ) ;
#19549 = CARTESIAN_POINT ( 'NONE',  ( -23.90000000000000568, 29.49999999999999645, 12.00000000000000000 ) ) ;
#19550 = EDGE_CURVE ( 'NONE', #230, #15957, #15812, .T. ) ;
#19551 = AXIS2_PLACEMENT_3D ( 'NONE', #10484, #14275, #8158 ) ;
#19552 = ADVANCED_FACE ( 'NONE', ( #17630 ), #19237, .T. ) ;
#19553 = CARTESIAN_POINT ( 'NONE',  ( 31.10231664966676846, -45.36128193761570770, 12.00000000000000000 ) ) ;
#19554 = ORIENTED_EDGE ( 'NONE', *, *, #2629, .T. ) ;
#19555 = ORIENTED_EDGE ( 'NONE', *, *, #13289, .F. ) ;
#19556 = DIRECTION ( 'NONE',  ( -1.000000000000000000, -0.000000000000000000, -0.000000000000000000 ) ) ;
#19557 = CARTESIAN_POINT ( 'NONE',  ( -7.685661446562381371, 5.583959896777970222, -12.00674201446023481 ) ) ;
#19558 = ORIENTED_EDGE ( 'NONE', *, *, #9989, .F. ) ;
#19559 = ORIENTED_EDGE ( 'NONE', *, *, #21903, .F. ) ;
#19560 = DIRECTION ( 'NONE',  ( -1.000000000000000000, -1.224606353822377258E-16, -0.000000000000000000 ) ) ;
#19561 = FACE_OUTER_BOUND ( 'NONE', #7450, .T. ) ;
#19562 = ORIENTED_EDGE ( 'NONE', *, *, #23419, .T. ) ;
#19563 = DIRECTION ( 'NONE',  ( 1.000000000000000000, -0.000000000000000000, 0.000000000000000000 ) ) ;
#19564 = AXIS2_PLACEMENT_3D ( 'NONE', #6582, #8256, #10084 ) ;
#19565 = VECTOR ( 'NONE', #8022, 999.9999999999998863 ) ;
#19566 = AXIS2_PLACEMENT_3D ( 'NONE', #9869, #18929, #2209 ) ;
#19567 = ORIENTED_EDGE ( 'NONE', *, *, #3321, .T. ) ;
#19568 = EDGE_CURVE ( 'NONE', #7789, #19098, #9941, .T. ) ;
#19569 = CARTESIAN_POINT ( 'NONE',  ( 71.96568270381689558, 7.420530141404717394E-15, 0.000000000000000000 ) ) ;
#19570 = PRODUCT ( 'Body', 'Body', '', ( #201 ) ) ;
#19571 = LINE ( 'NONE', #1153, #9469 ) ;
#19572 = AXIS2_PLACEMENT_3D ( 'NONE', #2322, #22695, #5984 ) ;
#19573 = CARTESIAN_POINT ( 'NONE',  ( -40.23082370883260239, 27.62204025492846071, -1.500000000000000000 ) ) ;
#19574 = DIRECTION ( 'NONE',  ( 0.7052211081716914798, 0.7089874389501492624, -0.000000000000000000 ) ) ;
#19575 = VERTEX_POINT ( 'NONE', #699 ) ;
#19576 = DIRECTION ( 'NONE',  ( -0.5000000000000034417, 1.060575238724904696E-16, -0.8660254037844367092 ) ) ;
#19577 = EDGE_CURVE ( 'NONE', #12085, #8138, #18315, .T. ) ;
#19578 = CARTESIAN_POINT ( 'NONE',  ( -28.99999999999999645, 29.50000000000000711, -1.500000000000000000 ) ) ;
#19579 = EDGE_CURVE ( 'NONE', #12687, #19120, #13619, .T. ) ;
#19580 = CARTESIAN_POINT ( 'NONE',  ( -28.99999999999999645, 29.50000000000000000, 14.00000000000000178 ) ) ;
#19581 = CARTESIAN_POINT ( 'NONE',  ( 5.871322893123449127, 8.081182679344781405, 6.359589141758142716 ) ) ;
#19582 = ORIENTED_EDGE ( 'NONE', *, *, #16741, .F. ) ;
#19583 = ORIENTED_EDGE ( 'NONE', *, *, #22736, .T. ) ;
#19584 = ORIENTED_EDGE ( 'NONE', *, *, #19300, .T. ) ;
#19585 = EDGE_LOOP ( 'NONE', ( #17507, #8472, #16376, #13981 ) ) ;
#19586 = VECTOR ( 'NONE', #13990, 1000.000000000000000 ) ;
#19587 = ORIENTED_EDGE ( 'NONE', *, *, #2089, .T. ) ;
#19588 = VECTOR ( 'NONE', #23088, 1000.000000000000000 ) ;
#19590 = AXIS2_PLACEMENT_3D ( 'NONE', #21081, #23045, #22676 ) ;
#19589 = FACE_OUTER_BOUND ( 'NONE', #19092, .T. ) ;
#19591 = AXIS2_PLACEMENT_3D ( 'NONE', #904, #2981, #781 ) ;
#19592 = CARTESIAN_POINT ( 'NONE',  ( 23.00000000000000000, -13.61176534793443338, -4.089617900950226925 ) ) ;
#19593 = CARTESIAN_POINT ( 'NONE',  ( 9.500000000000000000, 6.470877716354879437E-13, -5.206742014460234103 ) ) ;
#19594 = ORIENTED_EDGE ( 'NONE', *, *, #4917, .T. ) ;
#19595 = CARTESIAN_POINT ( 'NONE',  ( 29.00000000000000000, 29.50000000000000355, 12.00000000000000000 ) ) ;
#19596 = CARTESIAN_POINT ( 'NONE',  ( 20.85000000000000853, 15.03999999999999915, 25.00000000000000000 ) ) ;
#19597 = ORIENTED_EDGE ( 'NONE', *, *, #17903, .F. ) ;
#19598 = FACE_BOUND ( 'NONE', #2818, .T. ) ;
#19599 = DIRECTION ( 'NONE',  ( -1.000000000000000000, -0.000000000000000000, -0.000000000000000000 ) ) ;
#19600 = EDGE_CURVE ( 'NONE', #5846, #7241, #13987, .T. ) ;
#19601 = CARTESIAN_POINT ( 'NONE',  ( -7.685661446562381371, 5.583959896777970222, 6.006742014460233037 ) ) ;
#19602 = LINE ( 'NONE', #6665, #15158 ) ;
#19603 = CARTESIAN_POINT ( 'NONE',  ( 1.499999999999999556, 2.143131898507867804E-16, 6.000000000000000000 ) ) ;
#19604 = EDGE_CURVE ( 'NONE', #569, #5416, #3103, .T. ) ;
#19605 = LINE ( 'NONE', #10315, #21659 ) ;
#19606 = VECTOR ( 'NONE', #11036, 1000.000000000000000 ) ;
#19607 = CYLINDRICAL_SURFACE ( 'NONE', #3264, 15.00000000000000000 ) ;
#19608 = EDGE_CURVE ( 'NONE', #19153, #21270, #3236, .T. ) ;
#19609 = CARTESIAN_POINT ( 'NONE',  ( -5.365059087798940141, -7.384370330707086261, -7.933165578109187877 ) ) ;
#19610 = TOROIDAL_SURFACE ( 'NONE', #14511, 2.500000000000001776, 1.000000000000000000 ) ;
#19611 = AXIS2_PLACEMENT_3D ( 'NONE', #15098, #20726, #22678 ) ;
#19612 = ADVANCED_FACE ( 'NONE', ( #10540 ), #3360, .F. ) ;
#19613 = AXIS2_PLACEMENT_3D ( 'NONE', #15434, #4107, #21175 ) ;
#19614 = AXIS2_PLACEMENT_3D ( 'NONE', #3294, #20488, #16332 ) ;
#19615 = VECTOR ( 'NONE', #5404, 1000.000000000000000 ) ;
#19616 = DIRECTION ( 'NONE',  ( -1.000000000000000000, 0.000000000000000000, 0.000000000000000000 ) ) ;
#19617 = EDGE_LOOP ( 'NONE', ( #10394, #9937 ) ) ;
#19618 = ORIENTED_EDGE ( 'NONE', *, *, #7804, .T. ) ;
#19619 = CIRCLE ( 'NONE', #17643, 5.000000000000007994 ) ;
#19620 = AXIS2_PLACEMENT_3D ( 'NONE', #3907, #4034, #16480 ) ;
#19621 = ORIENTED_EDGE ( 'NONE', *, *, #443, .T. ) ;
#19622 = CARTESIAN_POINT ( 'NONE',  ( 693.7818939062881327, 933.4837211537982284, 1290.481724745928432 ) ) ;
#19623 = DIRECTION ( 'NONE',  ( 0.000000000000000000, -0.000000000000000000, 1.000000000000000000 ) ) ;
#19624 = ORIENTED_EDGE ( 'NONE', *, *, #13931, .T. ) ;
#19625 = DIRECTION ( 'NONE',  ( 1.000000000000000000, 0.000000000000000000, 0.000000000000000000 ) ) ;
#19626 = UNCERTAINTY_MEASURE_WITH_UNIT (LENGTH_MEASURE( 1.000000000000000082E-05 ), #8270, 'distance_accuracy_value', 'NONE');
#19627 = CARTESIAN_POINT ( 'NONE',  ( 2.599411561834574336, 8.617182949674106140, 100.5103153236600519 ) ) ;
#19629 = AXIS2_PLACEMENT_3D ( 'NONE', #382, #1958, #22032 ) ;
#19628 = DIRECTION ( 'NONE',  ( 0.000000000000000000, -0.000000000000000000, 1.000000000000000000 ) ) ;
#19630 = DIRECTION ( 'NONE',  ( -0.000000000000000000, -0.000000000000000000, -1.000000000000000000 ) ) ;
#19631 = AXIS2_PLACEMENT_3D ( 'NONE', #11927, #13646, #19138 ) ;
#19632 = CIRCLE ( 'NONE', #9079, 4.172000000000008590 ) ;
#19633 = EDGE_LOOP ( 'NONE', ( #11097, #14395, #21312, #5061, #16734, #19277 ) ) ;
#19634 = CONICAL_SURFACE ( 'NONE', #20010, 4.172000000000008590, 0.9599310885968742602 ) ;
#19635 = DIRECTION ( 'NONE',  ( -0.000000000000000000, -0.000000000000000000, 1.000000000000000000 ) ) ;
#19636 = ADVANCED_FACE ( 'NONE', ( #7254 ), #18355, .F. ) ;
#19637 = TOROIDAL_SURFACE ( 'NONE', #17274, 19.84999999999999787, 1.000000000000000000 ) ;
#19638 = PLANE ( 'NONE',  #16155 ) ;
#19639 = DIRECTION ( 'NONE',  ( -0.000000000000000000, -0.000000000000000000, 1.000000000000000000 ) ) ;
#19640 = ORIENTED_EDGE ( 'NONE', *, *, #22985, .T. ) ;
#19641 = CARTESIAN_POINT ( 'NONE',  ( -9.500000000000000000, -6.482511860946779655E-13, 6.206742014460234103 ) ) ;
#19642 = AXIS2_PLACEMENT_3D ( 'NONE', #5600, #16695, #10935 ) ;
#19643 = CARTESIAN_POINT ( 'NONE',  ( 0.000000000000000000, 15.03999999999999915, 27.00000000000000000 ) ) ;
#19644 =( REPRESENTATION_RELATIONSHIP ('NONE','NONE', #2851, #2057 ) REPRESENTATION_RELATIONSHIP_WITH_TRANSFORMATION ( #522 )SHAPE_REPRESENTATION_RELATIONSHIP( ) );
#19645 = DIRECTION ( 'NONE',  ( -1.000000000000000000, 0.000000000000000000, 0.000000000000000000 ) ) ;
#19646 = ADVANCED_FACE ( 'NONE', ( #20198 ), #10779, .F. ) ;
#19647 = ORIENTED_EDGE ( 'NONE', *, *, #22025, .T. ) ;
#19648 = ADVANCED_FACE ( 'NONE', ( #12382 ), #1297, .F. ) ;
#19649 = VERTEX_POINT ( 'NONE', #12742 ) ;
#19650 = ORIENTED_EDGE ( 'NONE', *, *, #6800, .T. ) ;
#19651 = VECTOR ( 'NONE', #16106, 1000.000000000000000 ) ;
#19652 = CARTESIAN_POINT ( 'NONE',  ( -9.500000000000211386, 3.086737114211961064, 2.959589141758143249 ) ) ;
#19653 = VECTOR ( 'NONE', #4691, 1000.000000000000000 ) ;
#19654 = ORIENTED_EDGE ( 'NONE', *, *, #11803, .T. ) ;
#19655 = VECTOR ( 'NONE', #2075, 1000.000000000000000 ) ;
#19656 = CARTESIAN_POINT ( 'NONE',  ( 12.50000000000000178, 5.755434930044642846E-15, -2.500000000000000000 ) ) ;
#19657 = CIRCLE ( 'NONE', #14985, 4.172000000000008590 ) ;
#19658 = CARTESIAN_POINT ( 'NONE',  ( 41.73082370883258108, -29.49999999999999645, 0.000000000000000000 ) ) ;
#19659 = CARTESIAN_POINT ( 'NONE',  ( 3.000000000000000888, 111.0000000000000000, 80.99999999999998579 ) ) ;
#19660 = CIRCLE ( 'NONE', #20416, 17.87500000001787726 ) ;
#19661 = CONICAL_SURFACE ( 'NONE', #7166, 1.999999999999994449, 1.029744258676653201 ) ;
#19662 = CARTESIAN_POINT ( 'NONE',  ( 40.23082370883258818, -29.49999999999999645, -1.500000000000000000 ) ) ;
#19663 = DIRECTION ( 'NONE',  ( 1.000000000000000000, 0.000000000000000000, -0.000000000000000000 ) ) ;
#19664 = CARTESIAN_POINT ( 'NONE',  ( 81.27272727272728048, 4.172000000000015696, 5.109226446042767468E-16 ) ) ;
#19665 = CARTESIAN_POINT ( 'NONE',  ( 1.500000000000001332, 0.000000000000000000, 0.000000000000000000 ) ) ;
#19666 = EDGE_CURVE ( 'NONE', #21154, #18241, #4973, .T. ) ;
#19667 = ORIENTED_EDGE ( 'NONE', *, *, #19834, .T. ) ;
#19668 = DIRECTION ( 'NONE',  ( -1.000000000000000000, 0.000000000000000000, 0.000000000000000000 ) ) ;
#19669 = ORIENTED_EDGE ( 'NONE', *, *, #5751, .T. ) ;
#19670 = CARTESIAN_POINT ( 'NONE',  ( -31.74999999999995737, 0.000000000000000000, 5.000000000000000888 ) ) ;
#19671 = LINE ( 'NONE', #6963, #19651 ) ;
#19672 = CARTESIAN_POINT ( 'NONE',  ( 5.378177448618336243, 1.193683371863418128E-15, 9.747164428915397139 ) ) ;
#19673 = LINE ( 'NONE', #23448, #23740 ) ;
#19674 = AXIS2_PLACEMENT_3D ( 'NONE', #10811, #18277, #5346 ) ;
#19675 = CIRCLE ( 'NONE', #15346, 8.000000000000003553 ) ;
#19676 = CARTESIAN_POINT ( 'NONE',  ( 23.00000000000000000, -0.09016380984455869829, -11.68615217844040721 ) ) ;
#19677 = EDGE_LOOP ( 'NONE', ( #1308, #15714, #17968, #4075, #19532 ) ) ;
#19678 = ADVANCED_FACE ( 'NONE', ( #6783 ), #18002, .T. ) ;
#19679 = CARTESIAN_POINT ( 'NONE',  ( -7.685661446562381371, 5.583959896777970222, 8.859589141758144493 ) ) ;
#19680 = ORIENTED_EDGE ( 'NONE', *, *, #18737, .F. ) ;
#19681 = CARTESIAN_POINT ( 'NONE',  ( 41.00000000000000000, -26.23076770084981391, 12.00000000000000000 ) ) ;
#19682 = ORIENTED_EDGE ( 'NONE', *, *, #5228, .T. ) ;
#19683 = CARTESIAN_POINT ( 'NONE',  ( 2.570122167802765922, 0.000000000000000000, 0.000000000000000000 ) ) ;
#19684 = CARTESIAN_POINT ( 'NONE',  ( 0.000000000000000000, 14.21257171757157245, 0.08908218613057176938 ) ) ;
#19685 = DIRECTION ( 'NONE',  ( 0.000000000000000000, 1.000000000000000000, 0.000000000000000000 ) ) ;
#19686 =( BOUNDED_SURFACE ( )  B_SPLINE_SURFACE ( 1, 2, ( 
 ( #19278, #9975, #733, #17314, #6214, #23052, #15348, #21226, #9851, #20984, #4530, #5974, #13653, #19146, #10094, #11936, #4273, #22567, #21090, #11438, #4390, #22820, #7899, #7776, #15213, #13539, #11676, #5852, #19402, #2562, #846, #15105, #22683, #13408, #13277, #20734, #20871, #17179, #2425, #4021, #4160, #9619, #11570, #12527, #23184, #21719, #21354, #6703, #6467, #1103, #4644, #14135, #19999, #21826, #12045, #14369, #3278, #8525, #8405, #2925, #5006, #3157, #15719, #5107, #10705, #18177, #3049, #19517, #10352, #8630, #17815, #2796, #6947, #15854, #15967, #12171, #10217, #23545, #23428, #21597, #6592, #8267, #4892, #13912, #17678, #979, #19774, #12304, #12420, #23315, #14023, #19652, #1219, #10581, #21469, #10470, #17931 ),
 ( #16083, #6827, #14257, #19880, #4762, #18046, #1344, #8768, #16216, #23676, #6898, #14611, #1922, #20474, #23895, #3763, #11050, #11171, #21948, #12659, #22309, #18288, #5587, #5354, #13017, #1572, #1471, #14837, #18645, #8884, #10924, #14477, #16321, #23776, #7399, #12779, #7048, #9239, #22196, #20239, #16686, #5232, #20127, #16431, #3403, #10819, #3516, #8986, #7174, #22081, #18396, #1691, #12893, #9115, #16563, #24018, #7293, #14733, #5469, #20349, #1817, #3633, #18529, #8842, #6550, #12124, #6781, #3114, #8484, #3012, #16280, #4847, #19601, #6663, #13986, #3233, #1065, #2877, #15929, #10430, #10778, #23390, #14210, #21898, #8590, #14094, #5072, #10662, #21549, #12380, #21674, #10538, #18000, #5183, #3359, #23744, #21430 ) ),
 .UNSPECIFIED., .F., .F., .F. ) 
 B_SPLINE_SURFACE_WITH_KNOTS ( ( 2, 2 ),
 ( 3, 2, 2, 2, 2, 2, 2, 2, 2, 2, 2, 2, 2, 2, 2, 2, 2, 2, 2, 2, 2, 2, 2, 2, 2, 2, 2, 2, 2, 2, 2, 2, 2, 2, 2, 2, 2, 2, 2, 2, 2, 2, 2, 2, 2, 2, 2, 2, 3 ),
 ( 0.000000000000000000, 1.000000000000000000 ),
 ( 0.000000000000000000, 0.02000000000000000042, 0.04000000000000000083, 0.05999999999999999778, 0.08000000000000000167, 0.1000000000000000056, 0.1199999999999999956, 0.1400000000000000133, 0.1600000000000000033, 0.1799999999999999933, 0.2000000000000000111, 0.2200000000000000011, 0.2399999999999999911, 0.2600000000000000089, 0.2800000000000000266, 0.2999999999999999889, 0.3200000000000000067, 0.3400000000000000244, 0.3599999999999999867, 0.3800000000000000044, 0.4000000000000000222, 0.4199999999999999845, 0.4400000000000000022, 0.4600000000000000200, 0.4799999999999999822, 0.5000000000000000000, 0.5200000000000000178, 0.5400000000000000355, 0.5600000000000000533, 0.5799999999999999600, 0.5999999999999999778, 0.6199999999999999956, 0.6400000000000000133, 0.6600000000000000311, 0.6800000000000000488, 0.6999999999999999556, 0.7199999999999999734, 0.7399999999999999911, 0.7600000000000000089, 0.7800000000000000266, 0.8000000000000000444, 0.8199999999999999512, 0.8399999999999999689, 0.8599999999999999867, 0.8800000000000000044, 0.9000000000000000222, 0.9200000000000000400, 0.9399999999999999467, 0.9500000000000000666 ),
 .UNSPECIFIED. ) 
 GEOMETRIC_REPRESENTATION_ITEM ( )  RATIONAL_B_SPLINE_SURFACE ( (
 ( 1.000000000000000000, 0.9510565162951535312, 1.000000000000000000, 0.9510565162951535312, 1.000000000000000000, 0.9510565162951535312, 1.000000000000000000, 0.9510565162951535312, 1.000000000000000000, 0.9510565162951535312, 1.000000000000000000, 0.9510565162951535312, 1.000000000000000000, 0.9510565162951535312, 1.000000000000000000, 0.9510565162951535312, 1.000000000000000000, 0.9510565162951535312, 1.000000000000000000, 0.9510565162951535312, 1.000000000000000000, 0.9510565162951535312, 1.000000000000000000, 0.9510565162951535312, 1.000000000000000000, 0.9510565162951535312, 1.000000000000000000, 0.9510565162951535312, 1.000000000000000000, 0.9510565162951535312, 1.000000000000000000, 0.9510565162951535312, 1.000000000000000000, 0.9510565162951535312, 1.000000000000000000, 0.9510565162951535312, 1.000000000000000000, 0.9510565162951535312, 1.000000000000000000, 0.9510565162951535312, 1.000000000000000000, 0.9510565162951535312, 1.000000000000000000, 0.9510565162951535312, 1.000000000000000000, 0.9510565162951535312, 1.000000000000000000, 0.9510565162951535312, 1.000000000000000000, 0.9510565162951535312, 1.000000000000000000, 0.9510565162951535312, 1.000000000000000000, 0.9510565162951535312, 1.000000000000000000, 0.9510565162951535312, 1.000000000000000000, 0.9510565162951535312, 1.000000000000000000, 0.9510565162951535312, 1.000000000000000000, 0.9510565162951535312, 1.000000000000000000, 0.9510565162951535312, 1.000000000000000000, 0.9510565162951535312, 1.000000000000000000, 0.9510565162951535312, 1.000000000000000000, 0.9510565162951535312, 1.000000000000000000, 0.9510565162951535312, 1.000000000000000000, 0.9510565162951535312, 1.000000000000000000, 0.9510565162951535312, 1.000000000000000000, 0.9510565162951535312, 1.000000000000000000, 0.9510565162951535312, 1.000000000000000000, 0.9510565162951535312, 1.000000000000000000, 0.9510565162951535312, 1.000000000000000000, 0.9510565162951535312, 1.000000000000000000, 0.9510565162951535312, 1.000000000000000000, 0.9510565162951535312, 1.000000000000000000, 0.9510565162951535312, 1.000000000000000000, 0.9510565162951535312, 1.000000000000000000, 0.9755282581475764880, 0.9755282581475768211),
 ( 1.000000000000000000, 0.9510565162951535312, 1.000000000000000000, 0.9510565162951535312, 1.000000000000000000, 0.9510565162951535312, 1.000000000000000000, 0.9510565162951535312, 1.000000000000000000, 0.9510565162951535312, 1.000000000000000000, 0.9510565162951535312, 1.000000000000000000, 0.9510565162951535312, 1.000000000000000000, 0.9510565162951535312, 1.000000000000000000, 0.9510565162951535312, 1.000000000000000000, 0.9510565162951535312, 1.000000000000000000, 0.9510565162951535312, 1.000000000000000000, 0.9510565162951535312, 1.000000000000000000, 0.9510565162951535312, 1.000000000000000000, 0.9510565162951535312, 1.000000000000000000, 0.9510565162951535312, 1.000000000000000000, 0.9510565162951535312, 1.000000000000000000, 0.9510565162951535312, 1.000000000000000000, 0.9510565162951535312, 1.000000000000000000, 0.9510565162951535312, 1.000000000000000000, 0.9510565162951535312, 1.000000000000000000, 0.9510565162951535312, 1.000000000000000000, 0.9510565162951535312, 1.000000000000000000, 0.9510565162951535312, 1.000000000000000000, 0.9510565162951535312, 1.000000000000000000, 0.9510565162951535312, 1.000000000000000000, 0.9510565162951535312, 1.000000000000000000, 0.9510565162951535312, 1.000000000000000000, 0.9510565162951535312, 1.000000000000000000, 0.9510565162951535312, 1.000000000000000000, 0.9510565162951535312, 1.000000000000000000, 0.9510565162951535312, 1.000000000000000000, 0.9510565162951535312, 1.000000000000000000, 0.9510565162951535312, 1.000000000000000000, 0.9510565162951535312, 1.000000000000000000, 0.9510565162951535312, 1.000000000000000000, 0.9510565162951535312, 1.000000000000000000, 0.9510565162951535312, 1.000000000000000000, 0.9510565162951535312, 1.000000000000000000, 0.9510565162951535312, 1.000000000000000000, 0.9510565162951535312, 1.000000000000000000, 0.9510565162951535312, 1.000000000000000000, 0.9510565162951535312, 1.000000000000000000, 0.9510565162951535312, 1.000000000000000000, 0.9510565162951535312, 1.000000000000000000, 0.9510565162951535312, 1.000000000000000000, 0.9510565162951535312, 1.000000000000000000, 0.9510565162951535312, 1.000000000000000000, 0.9755282581475764880, 0.9755282581475768211) ) ) 
 REPRESENTATION_ITEM ( '' )  SURFACE ( )  );
#19687 = AXIS2_PLACEMENT_3D ( 'NONE', #23060, #15484, #989 ) ;
#19688 = CONICAL_SURFACE ( 'NONE', #19276, 5.000000000000007994, 0.9599310885968855844 ) ;
#19689 = ORIENTED_EDGE ( 'NONE', *, *, #22569, .F. ) ;
#19690 = DIRECTION ( 'NONE',  ( -0.000000000000000000, -0.000000000000000000, -1.000000000000000000 ) ) ;
#19691 = EDGE_CURVE ( 'NONE', #12610, #15653, #18136, .T. ) ;
#19692 = ORIENTED_EDGE ( 'NONE', *, *, #448, .F. ) ;
#19693 = AXIS2_PLACEMENT_3D ( 'NONE', #17055, #354, #7766 ) ;
#19694 = ORIENTED_EDGE ( 'NONE', *, *, #320, .F. ) ;
#19695 = EDGE_CURVE ( 'NONE', #10068, #2874, #1166, .T. ) ;
#19696 = CARTESIAN_POINT ( 'NONE',  ( 89.17200000000002547, 0.000000000000000000, 0.000000000000000000 ) ) ;
#19697 = EDGE_LOOP ( 'NONE', ( #12568, #17408, #14594, #2095 ) ) ;
#19698 = DIRECTION ( 'NONE',  ( -1.000000000000000000, -0.000000000000000000, -0.000000000000000000 ) ) ;
#19699 = VECTOR ( 'NONE', #9093, 1000.000000000000000 ) ;
#19700 =( GEOMETRIC_REPRESENTATION_CONTEXT ( 3 ) GLOBAL_UNCERTAINTY_ASSIGNED_CONTEXT ( ( #14004 ) ) GLOBAL_UNIT_ASSIGNED_CONTEXT ( ( #10936, #18655, #18542 ) ) REPRESENTATION_CONTEXT ( 'NONE', 'WORKASPACE' ) );
#19701 = EDGE_CURVE ( 'NONE', #7578, #4470, #7760, .T. ) ;
#19702 = ORIENTED_EDGE ( 'NONE', *, *, #7649, .F. ) ;
#19703 = LINE ( 'NONE', #4578, #2031 ) ;
#19704 = ADVANCED_FACE ( 'NONE', ( #23503, #22156 ), #21899, .T. ) ;
#19705 = FACE_OUTER_BOUND ( 'NONE', #3470, .T. ) ;
#19706 = CARTESIAN_POINT ( 'NONE',  ( -35.99999999999994316, -60.00000000000000000, 0.000000000000000000 ) ) ;
#19707 = DIRECTION ( 'NONE',  ( 0.000000000000000000, -1.000000000000000000, 0.000000000000000000 ) ) ;
#19708 = ORIENTED_EDGE ( 'NONE', *, *, #9297, .F. ) ;
#19709 = CYLINDRICAL_SURFACE ( 'NONE', #22379, 4.249999999999996447 ) ;
#19710 = DIRECTION ( 'NONE',  ( 0.000000000000000000, 0.000000000000000000, -1.000000000000000000 ) ) ;
#19711 = CYLINDRICAL_SURFACE ( 'NONE', #5683, 9.500000000000000000 ) ;
#19712 = AXIS2_PLACEMENT_3D ( 'NONE', #11713, #9895, #17353 ) ;
#19713 = CARTESIAN_POINT ( 'NONE',  ( -5.871322893124554021, 8.081182679343978492, 8.759589141758141295 ) ) ;
#19714 = AXIS2_PLACEMENT_3D ( 'NONE', #19659, #4401, #11814 ) ;
#19715 = AXIS2_PLACEMENT_3D ( 'NONE', #738, #21359, #2683 ) ;
#19716 = AXIS2_PLACEMENT_3D ( 'NONE', #11072, #19036, #20867 ) ;
#19717 = ORIENTED_EDGE ( 'NONE', *, *, #10149, .T. ) ;
#19718 = DIRECTION ( 'NONE',  ( 0.7071067811865474617, 8.659560562354932858E-17, -0.7071067811865474617 ) ) ;
#19719 = EDGE_CURVE ( 'NONE', #23304, #2794, #11253, .T. ) ;
#19720 = DIRECTION ( 'NONE',  ( 0.000000000000000000, 0.000000000000000000, 1.000000000000000000 ) ) ;
#19721 = DIRECTION ( 'NONE',  ( -0.000000000000000000, 0.000000000000000000, 1.000000000000000000 ) ) ;
#19722 = ORIENTED_EDGE ( 'NONE', *, *, #4700, .F. ) ;
#19723 = DIRECTION ( 'NONE',  ( -0.000000000000000000, -0.000000000000000000, -1.000000000000000000 ) ) ;
#19724 = EDGE_CURVE ( 'NONE', #14, #5201, #3013, .T. ) ;
#19725 = AXIS2_PLACEMENT_3D ( 'NONE', #19810, #4678, #18215 ) ;
#19726 = CARTESIAN_POINT ( 'NONE',  ( -28.00000000000000355, -3.851859888774471706E-31, 12.00000000000000000 ) ) ;
#19727 = ORIENTED_EDGE ( 'NONE', *, *, #22164, .F. ) ;
#19728 = DIRECTION ( 'NONE',  ( 0.000000000000000000, 1.000000000000000000, 0.000000000000000000 ) ) ;
#19729 = FACE_OUTER_BOUND ( 'NONE', #3140, .T. ) ;
#19730 = ADVANCED_FACE ( 'NONE', ( #8843 ), #18245, .F. ) ;
#19732 = DIRECTION ( 'NONE',  ( -0.000000000000000000, -0.000000000000000000, -1.000000000000000000 ) ) ;
#19731 = AXIS2_PLACEMENT_3D ( 'NONE', #20136, #23681, #1699 ) ;
#19733 = CARTESIAN_POINT ( 'NONE',  ( 0.000000000000000000, 0.000000000000000000, -12.50000000000000000 ) ) ;
#19734 = CIRCLE ( 'NONE', #14238, 11.68650000001168721 ) ;
#19735 = FACE_OUTER_BOUND ( 'NONE', #23144, .T. ) ;
#19736 = AXIS2_PLACEMENT_3D ( 'NONE', #37, #7234, #7446 ) ;
#19737 = CARTESIAN_POINT ( 'NONE',  ( -14.51962751333974033, -3.765689428759031010, 8.721787840009202597 ) ) ;
#19738 = DIRECTION ( 'NONE',  ( 1.000000000000000000, 0.000000000000000000, 0.000000000000000000 ) ) ;
#19739 = DIRECTION ( 'NONE',  ( 0.000000000000000000, -0.000000000000000000, -1.000000000000000000 ) ) ;
#19740 = EDGE_LOOP ( 'NONE', ( #23051, #9301, #798, #11307, #9374, #16596 ) ) ;
#19741 = CARTESIAN_POINT ( 'NONE',  ( 70.21613547800127719, 5.000000000000015099, 0.000000000000000000 ) ) ;
#19742 = ORIENTED_EDGE ( 'NONE', *, *, #14383, .T. ) ;
#19743 = CARTESIAN_POINT ( 'NONE',  ( -8.680847955711007202, -5.923547351154968927E-13, 5.633165578109188942 ) ) ;
#19744 = AXIS2_PLACEMENT_3D ( 'NONE', #2144, #18991, #5921 ) ;
#19745 = ORIENTED_EDGE ( 'NONE', *, *, #9758, .T. ) ;
#19746 = DIRECTION ( 'NONE',  ( 0.9999982353878229535, -0.001878622165418357545, 0.000000000000000000 ) ) ;
#19747 = AXIS2_PLACEMENT_3D ( 'NONE', #5198, #10793, #6919 ) ;
#19748 = DIRECTION ( 'NONE',  ( 1.000000000000000000, 0.000000000000000000, 0.000000000000000000 ) ) ;
#19749 = AXIS2_PLACEMENT_3D ( 'NONE', #5062, #10529, #17989 ) ;
#19750 = VERTEX_POINT ( 'NONE', #23846 ) ;
#19751 = ORIENTED_EDGE ( 'NONE', *, *, #8473, .F. ) ;
#19752 = CARTESIAN_POINT ( 'NONE',  ( -29.00000000000000000, -29.49999999999999645, 0.000000000000000000 ) ) ;
#19753 = CARTESIAN_POINT ( 'NONE',  ( -5.871322893123450015, -8.081182679344781405, -5.359589141758144493 ) ) ;
#19754 = ADVANCED_FACE ( 'NONE', ( #7128 ), #2318, .F. ) ;
#19755 =( GEOMETRIC_REPRESENTATION_CONTEXT ( 3 ) GLOBAL_UNCERTAINTY_ASSIGNED_CONTEXT ( ( #10075 ) ) GLOBAL_UNIT_ASSIGNED_CONTEXT ( ( #19890, #1356, #14380 ) ) REPRESENTATION_CONTEXT ( 'NONE', 'WORKASPACE' ) );
#19756 = CARTESIAN_POINT ( 'NONE',  ( 40.23082370883260239, 29.49999999999999645, -3.000000000000000000 ) ) ;
#19757 = CARTESIAN_POINT ( 'NONE',  ( 14.51962751333974389, 3.765689428759029234, 8.721787840009197268 ) ) ;
#19758 = DIRECTION ( 'NONE',  ( 4.613626265895763066E-16, 1.000000000000000000, 0.000000000000000000 ) ) ;
#19759 = EDGE_CURVE ( 'NONE', #22524, #13479, #752, .T. ) ;
#19760 = ADVANCED_FACE ( 'NONE', ( #20308 ), #2332, .T. ) ;
#19761 = CARTESIAN_POINT ( 'NONE',  ( 24.75000000000000711, -29.50000000000000000, -2.224999999999995204 ) ) ;
#19762 = DIRECTION ( 'NONE',  ( -1.000000000000000000, 0.000000000000000000, 0.000000000000000000 ) ) ;
#19763 = AXIS2_PLACEMENT_3D ( 'NONE', #19684, #12210, #6734 ) ;
#19764 = DIRECTION ( 'NONE',  ( 1.000000000000000000, 0.000000000000000000, 0.000000000000000000 ) ) ;
#19765 = ORIENTED_EDGE ( 'NONE', *, *, #21700, .F. ) ;
#19766 = CARTESIAN_POINT ( 'NONE',  ( 5.378177448618336243, 0.000000000000000000, 0.000000000000000000 ) ) ;
#19767 = CARTESIAN_POINT ( 'NONE',  ( 5.000000000000000000, -4.685197434473820088, 9.540979117872439019E-15 ) ) ;
#19768 = DIRECTION ( 'NONE',  ( 0.000000000000000000, -1.000000000000000000, 0.000000000000000000 ) ) ;
#19769 = FACE_OUTER_BOUND ( 'NONE', #6286, .T. ) ;
#19770 = EDGE_LOOP ( 'NONE', ( #330, #360, #10338, #19063 ) ) ;
#19771 = CARTESIAN_POINT ( 'NONE',  ( 5.365059087798938364, 7.384370330707087149, -4.933165578109187877 ) ) ;
#19772 = ORIENTED_EDGE ( 'NONE', *, *, #20817, .F. ) ;
#19773 = ORIENTED_EDGE ( 'NONE', *, *, #19550, .T. ) ;
#19774 = CARTESIAN_POINT ( 'NONE',  ( -2.935661446561384391, -9.035036904804158553, 3.459589141758144137 ) ) ;
#19775 = CARTESIAN_POINT ( 'NONE',  ( 2.935661446561383503, 9.035036904804158553, 9.606742014460232681 ) ) ;
#19776 = CYLINDRICAL_SURFACE ( 'NONE', #18182, 9.000000000000000000 ) ;
#19777 = ORIENTED_EDGE ( 'NONE', *, *, #13728, .F. ) ;
#19778 = EDGE_CURVE ( 'NONE', #16640, #15261, #14396, .T. ) ;
#19779 = DIRECTION ( 'NONE',  ( 1.000000000000000000, 0.000000000000000000, -0.000000000000000000 ) ) ;
#19780 = CARTESIAN_POINT ( 'NONE',  ( -40.89823313241237912, -26.41789760203349502, 27.00000000000000000 ) ) ;
#19781 = CARTESIAN_POINT ( 'NONE',  ( 35.99999999999999289, -51.00000000000000711, 0.5000000000000004441 ) ) ;
#19782 = ORIENTED_EDGE ( 'NONE', *, *, #18150, .F. ) ;
#19783 = EDGE_CURVE ( 'NONE', #4241, #10216, #2215, .T. ) ;
#19784 = FACE_OUTER_BOUND ( 'NONE', #20332, .T. ) ;
#19785 = CARTESIAN_POINT ( 'NONE',  ( 20.99999999999999645, -29.50000000000000355, 11.50000000000000000 ) ) ;
#19786 = DIRECTION ( 'NONE',  ( -0.000000000000000000, -0.000000000000000000, -1.000000000000000000 ) ) ;
#19787 = ADVANCED_FACE ( 'NONE', ( #3585 ), #9638, .F. ) ;
#19788 = EDGE_CURVE ( 'NONE', #5633, #1485, #21239, .T. ) ;
#19789 = EDGE_CURVE ( 'NONE', #16948, #11149, #13673, .T. ) ;
#19790 = ORIENTED_EDGE ( 'NONE', *, *, #21804, .T. ) ;
#19791 = CARTESIAN_POINT ( 'NONE',  ( 74.87477361290781630, 7.420530141404717394E-15, 0.000000000000000000 ) ) ;
#19792 = ORIENTED_EDGE ( 'NONE', *, *, #11058, .F. ) ;
#19793 = DIRECTION ( 'NONE',  ( 0.000000000000000000, 0.000000000000000000, 1.000000000000000000 ) ) ;
#19794 = DIRECTION ( 'NONE',  ( -0.4828336235133057208, -0.8757121056631633760, 0.000000000000000000 ) ) ;
#19795 = CARTESIAN_POINT ( 'NONE',  ( 0.000000000000000000, -14.99147757894464306, 6.724999999999999645 ) ) ;
#19796 = CYLINDRICAL_SURFACE ( 'NONE', #10069, 1.000000000000000000 ) ;
#19797 = DIRECTION ( 'NONE',  ( 0.000000000000000000, 0.000000000000000000, -1.000000000000000000 ) ) ;
#19798 = ORIENTED_EDGE ( 'NONE', *, *, #9030, .F. ) ;
#19799 = CARTESIAN_POINT ( 'NONE',  ( -10.83999999999999986, -14.99147757894464306, 15.50000000000000000 ) ) ;
#19800 = VERTEX_POINT ( 'NONE', #280 ) ;
#19801 = CARTESIAN_POINT ( 'NONE',  ( 33.99999999999998579, -1.387778780781445676E-14, 9.500000000000000000 ) ) ;
#19802 = ORIENTED_EDGE ( 'NONE', *, *, #17328, .F. ) ;
#19803 = CARTESIAN_POINT ( 'NONE',  ( -2.682529543899159208, -8.255977015246598327, 4.033165578109189298 ) ) ;
#19804 = ORIENTED_EDGE ( 'NONE', *, *, #9460, .F. ) ;
#19805 = LINE ( 'NONE', #3077, #18206 ) ;
#19806 = EDGE_CURVE ( 'NONE', #747, #1952, #2086, .T. ) ;
#19807 = CARTESIAN_POINT ( 'NONE',  ( 82.14750088563508257, 7.420530141404717394E-15, 0.000000000000000000 ) ) ;
#19808 = CARTESIAN_POINT ( 'NONE',  ( 89.17200000000002547, 0.000000000000000000, 0.000000000000000000 ) ) ;
#19809 = ADVANCED_FACE ( 'NONE', ( #22704, #15374 ), #11697, .T. ) ;
#19810 = CARTESIAN_POINT ( 'NONE',  ( 65.85249911436491743, 7.562528597612068045E-15, 0.000000000000000000 ) ) ;
#19811 = EDGE_CURVE ( 'NONE', #11194, #12687, #5832, .T. ) ;
#19812 = CONICAL_SURFACE ( 'NONE', #3820, 4.172000000000008590, 0.9599310885968742602 ) ;
#19813 = VECTOR ( 'NONE', #4686, 1000.000000000000000 ) ;
#19814 = CARTESIAN_POINT ( 'NONE',  ( 6.809999908187194197E-13, -9.988891130263535700, -6.706742014460232326 ) ) ;
#19815 = ORIENTED_EDGE ( 'NONE', *, *, #12004, .F. ) ;
#19816 = ORIENTED_EDGE ( 'NONE', *, *, #15421, .F. ) ;
#19817 = CARTESIAN_POINT ( 'NONE',  ( -20.64923905428957340, -37.45138642374540439, 12.00000000000000000 ) ) ;
#19818 = ORIENTED_EDGE ( 'NONE', *, *, #17445, .T. ) ;
#19819 = DIRECTION ( 'NONE',  ( 0.000000000000000000, -1.000000000000000000, 0.000000000000000000 ) ) ;
#19820 = ORIENTED_EDGE ( 'NONE', *, *, #19099, .F. ) ;
#19821 = CARTESIAN_POINT ( 'NONE',  ( 40.89823313241237912, 26.41789760203348081, 27.00000000000000000 ) ) ;
#19822 = CARTESIAN_POINT ( 'NONE',  ( 43.99999999999999289, -51.00000000000000711, 0.5000000000000000000 ) ) ;
#19823 = FACE_OUTER_BOUND ( 'NONE', #3101, .T. ) ;
#19824 = ORIENTED_EDGE ( 'NONE', *, *, #17211, .F. ) ;
#19825 = DIRECTION ( 'NONE',  ( -1.000000000000000000, -1.224606353822377258E-16, -0.000000000000000000 ) ) ;
#19826 = CARTESIAN_POINT ( 'NONE',  ( -28.27483331787888332, -41.23752903419610050, 0.000000000000000000 ) ) ;
#19827 = CARTESIAN_POINT ( 'NONE',  ( 0.3000000000000020983, 0.000000000000000000, 14.72592346043842326 ) ) ;
#19828 = AXIS2_PLACEMENT_3D ( 'NONE', #18627, #13234, #16772 ) ;
#19829 = CIRCLE ( 'NONE', #12402, 49.99999999999998579 ) ;
#19830 = CARTESIAN_POINT ( 'NONE',  ( -5.871322893123450015, -8.081182679344781405, 3.359589141758143160 ) ) ;
#19831 = EDGE_LOOP ( 'NONE', ( #1983, #3542, #2257, #4603, #22437 ) ) ;
#19832 = ORIENTED_EDGE ( 'NONE', *, *, #5493, .F. ) ;
#19833 = CARTESIAN_POINT ( 'NONE',  ( 23.00000000000000000, 0.000000000000000000, 0.000000000000000000 ) ) ;
#19834 = EDGE_CURVE ( 'NONE', #758, #9485, #12050, .T. ) ;
#19835 = B_SPLINE_CURVE_WITH_KNOTS ( 'NONE', 3,
 ( #14589, #1319, #22061, #5449 ),
 .UNSPECIFIED., .F., .F.,
 ( 4, 4 ),
 ( 0.000000000000000000, 1.000000000000000000 ),
 .UNSPECIFIED. ) ;
#19836 = DIRECTION ( 'NONE',  ( 0.000000000000000000, -0.9096319953545137782, -0.4154150130018967602 ) ) ;
#19837 = DIRECTION ( 'NONE',  ( 1.000000000000000000, 0.000000000000000000, 0.000000000000000000 ) ) ;
#19838 = EDGE_LOOP ( 'NONE', ( #10064, #34 ) ) ;
#19839 = CARTESIAN_POINT ( 'NONE',  ( -16.68617496892349905, -7.233372502334341370, -6.175747996014760766 ) ) ;
#19840 = CYLINDRICAL_SURFACE ( 'NONE', #1679, 20.85000000000000497 ) ;
#19841 = CARTESIAN_POINT ( 'NONE',  ( 41.73082370883260239, 27.62204025492843940, -1.500000000000000000 ) ) ;
#19842 = ORIENTED_EDGE ( 'NONE', *, *, #11026, .F. ) ;
#19843 = LINE ( 'NONE', #19950, #16198 ) ;
#19844 = CARTESIAN_POINT ( 'NONE',  ( -9.499999999999790390, -3.086737114213257804, 7.159589141758144315 ) ) ;
#19845 = DIRECTION ( 'NONE',  ( -0.000000000000000000, -0.000000000000000000, -1.000000000000000000 ) ) ;
#19846 = DIRECTION ( 'NONE',  ( -1.000000000000000000, -1.224606353822377258E-16, -0.000000000000000000 ) ) ;
#19847 = CARTESIAN_POINT ( 'NONE',  ( -41.99999999999999289, 25.93535998569253920, 27.00000000000000000 ) ) ;
#19848 = CARTESIAN_POINT ( 'NONE',  ( 16.99687406587155891, -7.923972684219720009, -5.245599057861367598 ) ) ;
#19849 = DIRECTION ( 'NONE',  ( 0.5735764363510427177, -0.8191520442889941300, 1.003171929053527705E-16 ) ) ;
#19850 = DIRECTION ( 'NONE',  ( -1.000000000000000000, -0.000000000000000000, -0.000000000000000000 ) ) ;
#19851 = EDGE_CURVE ( 'NONE', #16191, #19878, #387, .T. ) ;
#19852 = ORIENTED_EDGE ( 'NONE', *, *, #2010, .F. ) ;
#19853 = DIRECTION ( 'NONE',  ( 0.000000000000000000, 0.000000000000000000, 1.000000000000000000 ) ) ;
#19854 = ORIENTED_EDGE ( 'NONE', *, *, #1883, .T. ) ;
#19855 = EDGE_CURVE ( 'NONE', #13001, #7696, #10112, .T. ) ;
#19856 = DIRECTION ( 'NONE',  ( 0.000000000000000000, 0.000000000000000000, 1.000000000000000000 ) ) ;
#19857 = DIRECTION ( 'NONE',  ( -1.000000000000000000, 0.000000000000000000, 0.000000000000000000 ) ) ;
#19858 = ORIENTED_EDGE ( 'NONE', *, *, #5797, .F. ) ;
#19859 = VERTEX_POINT ( 'NONE', #9875 ) ;
#19860 = ADVANCED_FACE ( 'NONE', ( #17084 ), #7794, .T. ) ;
#19861 = LINE ( 'NONE', #10555, #7973 ) ;
#19862 = CARTESIAN_POINT ( 'NONE',  ( 5.871322893124553133, -8.081182679343980269, -3.759589141758144404 ) ) ;
#19863 = CARTESIAN_POINT ( 'NONE',  ( 0.9681541731161901199, 8.949668379605448365, 101.8463591495539333 ) ) ;
#19864 = DIRECTION ( 'NONE',  ( 0.000000000000000000, 0.000000000000000000, 1.000000000000000000 ) ) ;
#19865 = VERTEX_POINT ( 'NONE', #4417 ) ;
#19866 = CARTESIAN_POINT ( 'NONE',  ( 41.73082370883257397, -27.62204025492843940, -1.500000000000000000 ) ) ;
#19867 = AXIS2_PLACEMENT_3D ( 'NONE', #16041, #20082, #1645 ) ;
#19868 = DIRECTION ( 'NONE',  ( 0.000000000000000000, 0.000000000000000000, 1.000000000000000000 ) ) ;
#19869 = DIRECTION ( 'NONE',  ( 1.000000000000000000, 0.000000000000000000, 0.000000000000000000 ) ) ;
#19870 = DIRECTION ( 'NONE',  ( -1.000000000000000000, -1.224606353822377258E-16, -0.000000000000000000 ) ) ;
#19871 = CARTESIAN_POINT ( 'NONE',  ( 33.99999999999998579, -1.387778780781445676E-14, 11.00000000000000000 ) ) ;
#19872 = FACE_BOUND ( 'NONE', #4906, .T. ) ;
#19873 = CARTESIAN_POINT ( 'NONE',  ( -1.999999999999996669, -45.00000000000000000, -8.673617379884035472E-16 ) ) ;
#19874 = ORIENTED_EDGE ( 'NONE', *, *, #9392, .T. ) ;
#19875 = CYLINDRICAL_SURFACE ( 'NONE', #900, 1.000000000000000000 ) ;
#19877 = ADVANCED_FACE ( 'NONE', ( #11830 ), #17455, .T. ) ;
#19876 = CARTESIAN_POINT ( 'NONE',  ( 6.809999908187194197E-13, -9.988891130263535700, -10.70674201446023233 ) ) ;
#19878 = VERTEX_POINT ( 'NONE', #23572 ) ;
#19879 = EDGE_LOOP ( 'NONE', ( #3569, #7756, #17993, #12843 ) ) ;
#19880 = CARTESIAN_POINT ( 'NONE',  ( 5.871322893124553133, -8.081182679343980269, 12.90674201446023517 ) ) ;
#19881 = EDGE_CURVE ( 'NONE', #2518, #7729, #15, .T. ) ;
#19882 = CARTESIAN_POINT ( 'NONE',  ( -9.499999999999790390, -3.086737114213257804, 6.306742014460231971 ) ) ;
#19883 = EDGE_CURVE ( 'NONE', #9464, #569, #6358, .T. ) ;
#19884 = ORIENTED_EDGE ( 'NONE', *, *, #10366, .T. ) ;
#19885 = DIRECTION ( 'NONE',  ( -1.000000000000000000, -0.000000000000000000, -0.000000000000000000 ) ) ;
#19886 = AXIS2_PLACEMENT_3D ( 'NONE', #2449, #18936, #6118 ) ;
#19887 = DIRECTION ( 'NONE',  ( 0.000000000000000000, -0.9096319953545137782, -0.4154150130018965936 ) ) ;
#19888 = DIRECTION ( 'NONE',  ( -1.000000000000000000, -1.224606353822377258E-16, -0.000000000000000000 ) ) ;
#19889 = DIRECTION ( 'NONE',  ( -1.000000000000000000, 0.000000000000000000, 0.000000000000000000 ) ) ;
#19890 =( LENGTH_UNIT ( ) NAMED_UNIT ( * ) SI_UNIT ( .MILLI., .METRE. ) );
#19891 = DIRECTION ( 'NONE',  ( -1.000000000000000000, 0.000000000000000000, 0.000000000000000000 ) ) ;
#19892 = DIRECTION ( 'NONE',  ( 1.000000000000000000, 1.224606353822377258E-16, 0.000000000000000000 ) ) ;
#19893 = ORIENTED_EDGE ( 'NONE', *, *, #21367, .F. ) ;
#19894 = ORIENTED_EDGE ( 'NONE', *, *, #1914, .F. ) ;
#19895 = FACE_OUTER_BOUND ( 'NONE', #5324, .T. ) ;
#19896 = PRODUCT_RELATED_PRODUCT_CATEGORY ( 'part', '', ( #13079 ) ) ;
#19897 = DIRECTION ( 'NONE',  ( 0.000000000000000000, -1.000000000000000000, 0.000000000000000000 ) ) ;
#19898 = LINE ( 'NONE', #23207, #8122 ) ;
#19899 = ADVANCED_FACE ( 'NONE', ( #17565 ), #10489, .F. ) ;
#19900 = MECHANICAL_DESIGN_GEOMETRIC_PRESENTATION_REPRESENTATION (  '', ( #14055 ), #20670 ) ;
#19901 = CARTESIAN_POINT ( 'NONE',  ( 23.00000000000000000, 2.967071445750139702, -17.62702788437271550 ) ) ;
#19902 = VERTEX_POINT ( 'NONE', #21739 ) ;
#19903 = CARTESIAN_POINT ( 'NONE',  ( 88.54545454545454675, 4.172000000000015696, 5.109226446042767468E-16 ) ) ;
#19904 = VERTEX_POINT ( 'NONE', #3173 ) ;
#19905 = CARTESIAN_POINT ( 'NONE',  ( 5.000000000000000000, -4.685197434473820088, 9.540979117872439019E-15 ) ) ;
#19906 = ORIENTED_EDGE ( 'NONE', *, *, #14141, .T. ) ;
#19907 = CARTESIAN_POINT ( 'NONE',  ( -2.024999999999999911, -45.00000000000000000, -27.00000000000000000 ) ) ;
#19908 = EDGE_CURVE ( 'NONE', #2673, #6921, #13631, .T. ) ;
#19909 = CARTESIAN_POINT ( 'NONE',  ( 0.000000000000000000, -45.00000000000000000, -2.974999999999996092 ) ) ;
#19910 = EDGE_CURVE ( 'NONE', #17944, #16608, #9724, .T. ) ;
#19911 = ORIENTED_EDGE ( 'NONE', *, *, #23165, .T. ) ;
#19912 = CARTESIAN_POINT ( 'NONE',  ( 41.99999999999997158, -25.22443390181681622, -1.500000000000000000 ) ) ;
#19913 = CARTESIAN_POINT ( 'NONE',  ( 14.51962751333974389, 3.765689428759029234, 27.00000000000000000 ) ) ;
#19914 = CARTESIAN_POINT ( 'NONE',  ( 0.000000000000000000, 5.985147671565880678, -12.89120389306408754 ) ) ;
#19915 = DIRECTION ( 'NONE',  ( 0.5735764363510427177, -0.8191520442889941300, 1.003171929053527705E-16 ) ) ;
#19917 = ORIENTED_EDGE ( 'NONE', *, *, #183, .F. ) ;
#19916 = VECTOR ( 'NONE', #6295, 1000.000000000000000 ) ;
#19918 = LINE ( 'NONE', #10264, #20084 ) ;
#19919 = CARTESIAN_POINT ( 'NONE',  ( -9.499999999999790390, -3.086737114213257804, -4.306742014460233747 ) ) ;
#19920 = ORIENTED_EDGE ( 'NONE', *, *, #10651, .T. ) ;
#19921 = EDGE_LOOP ( 'NONE', ( #1167, #17489, #16324, #6134 ) ) ;
#19922 = DIRECTION ( 'NONE',  ( -1.000000000000000000, 0.000000000000000000, 0.000000000000000000 ) ) ;
#19923 = CARTESIAN_POINT ( 'NONE',  ( 0.000000000000000000, -15.03999999999999915, 27.00000000000000000 ) ) ;
#19924 = EDGE_CURVE ( 'NONE', #9530, #16881, #15972, .T. ) ;
#19925 = VERTEX_POINT ( 'NONE', #19901 ) ;
#19926 = DIRECTION ( 'NONE',  ( -0.000000000000000000, -0.000000000000000000, -1.000000000000000000 ) ) ;
#19927 = CARTESIAN_POINT ( 'NONE',  ( -23.85000000000000497, 15.03999999999999915, 27.00000000000000000 ) ) ;
#19928 = AXIS2_PLACEMENT_3D ( 'NONE', #6605, #17697, #1234 ) ;
#19929 = ORIENTED_EDGE ( 'NONE', *, *, #15324, .F. ) ;
#19930 = CARTESIAN_POINT ( 'NONE',  ( -30.68762588338048403, 45.64284848299540442, -3.000000000000000000 ) ) ;
#19931 = CARTESIAN_POINT ( 'NONE',  ( 40.77574956473004164, -27.49633847812775755, 12.00000000000000000 ) ) ;
#19932 = EDGE_CURVE ( 'NONE', #4776, #23202, #10601, .T. ) ;
#19933 = CARTESIAN_POINT ( 'NONE',  ( 0.000000000000000000, 0.000000000000000000, 53.00000000000000000 ) ) ;
#19934 = EDGE_CURVE ( 'NONE', #11737, #18644, #22220, .T. ) ;
#19935 = VECTOR ( 'NONE', #10915, 1000.000000000000000 ) ;
#19936 = CARTESIAN_POINT ( 'NONE',  ( -39.00000000000000000, 28.80990663662251450, 12.00000000000000000 ) ) ;
#19937 = VERTEX_POINT ( 'NONE', #1368 ) ;
#19938 = VERTEX_POINT ( 'NONE', #15746 ) ;
#19939 = LINE ( 'NONE', #1417, #15849 ) ;
#19940 = DIRECTION ( 'NONE',  ( -0.000000000000000000, -0.000000000000000000, -1.000000000000000000 ) ) ;
#19941 = ORIENTED_EDGE ( 'NONE', *, *, #3499, .T. ) ;
#19942 = CIRCLE ( 'NONE', #23058, 4.999999999999997335 ) ;
#19943 = ORIENTED_EDGE ( 'NONE', *, *, #22646, .T. ) ;
#19944 = CARTESIAN_POINT ( 'NONE',  ( 28.73477696352899713, 42.73830357953205095, 0.000000000000000000 ) ) ;
#19945 = FACE_OUTER_BOUND ( 'NONE', #364, .T. ) ;
#19946 = CIRCLE ( 'NONE', #9789, 1.999999999999994449 ) ;
#19947 = CARTESIAN_POINT ( 'NONE',  ( 33.24999999999999289, 29.50000000000000000, 14.00000000000000178 ) ) ;
#19948 = VECTOR ( 'NONE', #5538, 1000.000000000000000 ) ;
#19949 = VERTEX_POINT ( 'NONE', #23209 ) ;
#19950 = CARTESIAN_POINT ( 'NONE',  ( -41.99999999999999289, 1.163414459189984894E-15, -9.499999999999994671 ) ) ;
#19951 = CYLINDRICAL_SURFACE ( 'NONE', #14521, 6.050000000006050982 ) ;
#19952 = B_SPLINE_CURVE_WITH_KNOTS ( 'NONE', 3,
 ( #13034, #5125, #10838, #7312 ),
 .UNSPECIFIED., .F., .F.,
 ( 4, 4 ),
 ( 0.000000000000000000, 1.000000000000000000 ),
 .UNSPECIFIED. ) ;
#19953 = CARTESIAN_POINT ( 'NONE',  ( 78.94340820527399671, 7.562528597612068045E-15, 0.000000000000000000 ) ) ;
#19954 = LINE ( 'NONE', #1298, #8990 ) ;
#19955 = DIRECTION ( 'NONE',  ( -0.5735764363510519326, 0.8191520442889876907, 1.003171929053519816E-16 ) ) ;
#19956 = CARTESIAN_POINT ( 'NONE',  ( 68.76159002345582394, -5.000000000000000000, 6.123233995736775157E-16 ) ) ;
#19957 = CARTESIAN_POINT ( 'NONE',  ( -34.00000000000000000, -3.851859888774471706E-31, 12.00000000000000000 ) ) ;
#19958 = EDGE_CURVE ( 'NONE', #5616, #16538, #1002, .T. ) ;
#19959 = EDGE_CURVE ( 'NONE', #18301, #14710, #2699, .T. ) ;
#19960 = ORIENTED_EDGE ( 'NONE', *, *, #7304, .T. ) ;
#19961 = CARTESIAN_POINT ( 'NONE',  ( -7.022953521754877748, -5.102474405760673015, 11.83316557810918823 ) ) ;
#19962 = EDGE_LOOP ( 'NONE', ( #21141, #14157, #9476, #12047, #9563, #9065, #12125, #1512, #7024, #21524, #3990, #21482, #15893, #13120, #2763 ) ) ;
#19963 = AXIS2_PLACEMENT_3D ( 'NONE', #1913, #2021, #9694 ) ;
#19964 = AXIS2_PLACEMENT_3D ( 'NONE', #3794, #17185, #2070 ) ;
#19965 = AXIS2_PLACEMENT_3D ( 'NONE', #20725, #16580, #15097 ) ;
#19966 = PRODUCT_DEFINITION_SHAPE ( 'NONE', 'NONE',  #24105 ) ;
#19967 = CIRCLE ( 'NONE', #17616, 4.249999999999993783 ) ;
#19968 = PRODUCT_CONTEXT ( 'NONE', #4825, 'mechanical' ) ;
#19969 = AXIS2_PLACEMENT_3D ( 'NONE', #21520, #4690, #1399 ) ;
#19970 = FACE_BOUND ( 'NONE', #4880, .T. ) ;
#19971 = CIRCLE ( 'NONE', #13329, 5.000000000000000888 ) ;
#19972 = ORIENTED_EDGE ( 'NONE', *, *, #448, .T. ) ;
#19973 = CARTESIAN_POINT ( 'NONE',  ( 0.000000000000000000, 4.685197434473818312, -1.301042606982605321E-15 ) ) ;
#19974 = CARTESIAN_POINT ( 'NONE',  ( -2.935661446561384391, -9.035036904804158553, -9.459589141758144137 ) ) ;
#19975 = CARTESIAN_POINT ( 'NONE',  ( 0.000000000000000000, 0.000000000000000000, 0.000000000000000000 ) ) ;
#19976 = DIRECTION ( 'NONE',  ( -1.000000000000000000, -0.000000000000000000, -0.000000000000000000 ) ) ;
#19977 = DIRECTION ( 'NONE',  ( -1.000000000000000000, 0.000000000000000000, 0.000000000000000000 ) ) ;
#19978 = ADVANCED_FACE ( 'NONE', ( #8788 ), #8540, .F. ) ;
#19979 = CARTESIAN_POINT ( 'NONE',  ( 0.000000000000000000, 0.000000000000000000, 12.50000000000000000 ) ) ;
#19980 = DIRECTION ( 'NONE',  ( 1.000000000000000000, 0.000000000000000000, 0.000000000000000000 ) ) ;
#19981 = CONICAL_SURFACE ( 'NONE', #4809, 9.500000000000000000, 0.7853981633974500554 ) ;
#19982 = EDGE_CURVE ( 'NONE', #11172, #21057, #23072, .T. ) ;
#19983 = CIRCLE ( 'NONE', #17636, 4.172000000000008590 ) ;
#19984 = CARTESIAN_POINT ( 'NONE',  ( -9.500000000000000000, -6.482511860946779655E-13, -11.05958914175814556 ) ) ;
#19985 = DIRECTION ( 'NONE',  ( 0.000000000000000000, 0.000000000000000000, 1.000000000000000000 ) ) ;
#19986 = AXIS2_PLACEMENT_3D ( 'NONE', #8477, #15198, #2870 ) ;
#19987 = FACE_OUTER_BOUND ( 'NONE', #11252, .T. ) ;
#19988 = CARTESIAN_POINT ( 'NONE',  ( 15.09475045435787877, 4.494086555308248521, 8.407297576120603466 ) ) ;
#19989 = CIRCLE ( 'NONE', #13349, 5.000000000000007994 ) ;
#19990 = EDGE_CURVE ( 'NONE', #3826, #7831, #21374, .T. ) ;
#19991 = DIRECTION ( 'NONE',  ( 0.000000000000000000, 0.000000000000000000, 1.000000000000000000 ) ) ;
#19992 = EDGE_LOOP ( 'NONE', ( #17582, #23820, #4055, #9847 ) ) ;
#19993 = FACE_OUTER_BOUND ( 'NONE', #14842, .T. ) ;
#19994 = EDGE_CURVE ( 'NONE', #21048, #14261, #1124, .T. ) ;
#19995 = AXIS2_PLACEMENT_3D ( 'NONE', #13600, #20574, #15798 ) ;
#19996 = DIRECTION ( 'NONE',  ( -1.000000000000000000, -1.224606353822377258E-16, -0.000000000000000000 ) ) ;
#19997 = ORIENTED_EDGE ( 'NONE', *, *, #7778, .T. ) ;
#19998 = ORIENTED_EDGE ( 'NONE', *, *, #20971, .F. ) ;
#19999 = CARTESIAN_POINT ( 'NONE',  ( -7.685661446562381371, 5.583959896777970222, 6.859589141758143604 ) ) ;
#20000 = CARTESIAN_POINT ( 'NONE',  ( 6.809999908187194197E-13, -9.988891130263535700, 4.706742014460233214 ) ) ;
#20001 = EDGE_LOOP ( 'NONE', ( #15401, #22053, #8245 ) ) ;
#20002 = ORIENTED_EDGE ( 'NONE', *, *, #13534, .T. ) ;
#20003 = DIRECTION ( 'NONE',  ( -0.000000000000000000, -0.000000000000000000, 1.000000000000000000 ) ) ;
#20004 = DIRECTION ( 'NONE',  ( 0.000000000000000000, 0.000000000000000000, -1.000000000000000000 ) ) ;
#20005 = AXIS2_PLACEMENT_3D ( 'NONE', #17142, #15547, #17401 ) ;
#20006 = CIRCLE ( 'NONE', #9444, 5.000000000000007994 ) ;
#20007 = CARTESIAN_POINT ( 'NONE',  ( -1.749335460929532182, -9.337549220493269075, 3.500000000000028866 ) ) ;
#20008 = DIRECTION ( 'NONE',  ( 0.000000000000000000, 1.000000000000000000, -0.000000000000000000 ) ) ;
#20009 = AXIS2_PLACEMENT_3D ( 'NONE', #4841, #12372, #8712 ) ;
#20010 = AXIS2_PLACEMENT_3D ( 'NONE', #1776, #18719, #22267 ) ;
#20011 = AXIS2_PLACEMENT_3D ( 'NONE', #18808, #33, #5872 ) ;
#20012 = DIRECTION ( 'NONE',  ( -0.000000000000000000, -0.000000000000000000, -1.000000000000000000 ) ) ;
#20013 = CARTESIAN_POINT ( 'NONE',  ( 33.99999999999998579, -1.387778780781445676E-14, 10.49999999999999822 ) ) ;
#20014 = EDGE_CURVE ( 'NONE', #12041, #22524, #11266, .T. ) ;
#20015 = AXIS2_PLACEMENT_3D ( 'NONE', #23196, #11685, #741 ) ;
#20016 = ORIENTED_EDGE ( 'NONE', *, *, #19323, .F. ) ;
#20017 = EDGE_CURVE ( 'NONE', #8481, #21886, #3068, .T. ) ;
#20018 = DIRECTION ( 'NONE',  ( -0.5735764363510519326, 0.8191520442889876907, 1.003171929053519816E-16 ) ) ;
#20019 = CARTESIAN_POINT ( 'NONE',  ( -34.00000000000000000, -4.999999999999999112, 11.00000000000000000 ) ) ;
#20020 = CARTESIAN_POINT ( 'NONE',  ( -9.499999999999783284, -3.086737114213268018, -11.15958914175814698 ) ) ;
#20021 = AXIS2_PLACEMENT_3D ( 'NONE', #2584, #23070, #8290 ) ;
#20022 = LINE ( 'NONE', #12801, #18702 ) ;
#20023 = CARTESIAN_POINT ( 'NONE',  ( 5.365059087799946447, -7.384370330706356178, -8.333165578109190008 ) ) ;
#20024 = VECTOR ( 'NONE', #2244, 1000.000000000000000 ) ;
#20025 = DIRECTION ( 'NONE',  ( -1.000000000000000000, -1.224606353822377258E-16, -0.000000000000000000 ) ) ;
#20026 = AXIS2_PLACEMENT_3D ( 'NONE', #673, #15526, #17603 ) ;
#20027 = VERTEX_POINT ( 'NONE', #11955 ) ;
#20028 = CARTESIAN_POINT ( 'NONE',  ( -31.74999999999995737, 6.123233995736767268E-16, -5.000000000000000888 ) ) ;
#20029 = AXIS2_PLACEMENT_3D ( 'NONE', #15629, #21277, #6632 ) ;
#20030 = ORIENTED_EDGE ( 'NONE', *, *, #23123, .F. ) ;
#20031 = CONICAL_SURFACE ( 'NONE', #19969, 1.499999999999999556, 0.7853981633974457255 ) ;
#20032 = CARTESIAN_POINT ( 'NONE',  ( -8.680847955711007202, -5.923547351154968927E-13, 3.633165578109188054 ) ) ;
#20033 = CIRCLE ( 'NONE', #9473, 1.000000000000000000 ) ;
#20034 = CIRCLE ( 'NONE', #1722, 4.999999999999997335 ) ;
#20035 = EDGE_LOOP ( 'NONE', ( #12150, #1491, #18722, #17605, #15093 ) ) ;
#20036 = CARTESIAN_POINT ( 'NONE',  ( 41.49999999999999289, 27.79189783386526358, -27.00000000000000000 ) ) ;
#20037 = PLANE ( 'NONE',  #9892 ) ;
#20038 = CARTESIAN_POINT ( 'NONE',  ( -9.499999999999790390, -3.086737114213257804, -3.159589141758143871 ) ) ;
#20039 = DIRECTION ( 'NONE',  ( 0.000000000000000000, 0.000000000000000000, 1.000000000000000000 ) ) ;
#20040 = EDGE_LOOP ( 'NONE', ( #11052, #1651, #6497, #7981 ) ) ;
#20041 = DIRECTION ( 'NONE',  ( -0.000000000000000000, 1.000000000000000000, 1.224646799147353207E-16 ) ) ;
#20042 = DIRECTION ( 'NONE',  ( 0.000000000000000000, 0.000000000000000000, 1.000000000000000000 ) ) ;
#20043 = EDGE_CURVE ( 'NONE', #2834, #13441, #1943, .T. ) ;
#20044 = CARTESIAN_POINT ( 'NONE',  ( 9.500000000000000000, 6.470877716354879437E-13, -12.05958914175814378 ) ) ;
#20045 = ORIENTED_EDGE ( 'NONE', *, *, #8444, .F. ) ;
#20046 = CIRCLE ( 'NONE', #15745, 11.68650000001168721 ) ;
#20047 = ORIENTED_EDGE ( 'NONE', *, *, #4959, .T. ) ;
#20048 = LINE ( 'NONE', #21997, #16530 ) ;
#20049 = DIRECTION ( 'NONE',  ( 1.000000000000000000, 0.000000000000000000, 0.000000000000000000 ) ) ;
#20050 = ADVANCED_FACE ( 'NONE', ( #4663 ), #3656, .T. ) ;
#20051 = EDGE_CURVE ( 'NONE', #14543, #20252, #7014, .T. ) ;
#20052 = VECTOR ( 'NONE', #19922, 1000.000000000000000 ) ;
#20053 = ORIENTED_EDGE ( 'NONE', *, *, #6120, .T. ) ;
#20054 = CARTESIAN_POINT ( 'NONE',  ( 0.000000000000000000, 0.000000000000000000, 0.000000000000000000 ) ) ;
#20055 = CARTESIAN_POINT ( 'NONE',  ( 0.000000000000000000, 0.000000000000000000, 11.24716442891539714 ) ) ;
#20056 = CARTESIAN_POINT ( 'NONE',  ( 0.000000000000000000, 17.02535186363803632, 5.445458559199173543 ) ) ;
#20057 = ORIENTED_EDGE ( 'NONE', *, *, #10686, .T. ) ;
#20058 = DIRECTION ( 'NONE',  ( 0.000000000000000000, -1.000000000000000000, 0.000000000000000000 ) ) ;
#20059 = DIRECTION ( 'NONE',  ( -1.000000000000000000, -0.000000000000000000, -0.000000000000000000 ) ) ;
#20060 = CARTESIAN_POINT ( 'NONE',  ( -23.85000000000000142, 15.03999999999999737, 2.200000000000000178 ) ) ;
#20061 = CARTESIAN_POINT ( 'NONE',  ( 2.935661446562616295, -9.035036904803758873, 3.659589141758142983 ) ) ;
#20062 =( GEOMETRIC_REPRESENTATION_CONTEXT ( 3 ) GLOBAL_UNCERTAINTY_ASSIGNED_CONTEXT ( ( #15194 ) ) GLOBAL_UNIT_ASSIGNED_CONTEXT ( ( #10487, #10600, #6356 ) ) REPRESENTATION_CONTEXT ( 'NONE', 'WORKASPACE' ) );
#20063 = CIRCLE ( 'NONE', #4484, 10.00000000000000533 ) ;
#20064 = VECTOR ( 'NONE', #23399, 1000.000000000000000 ) ;
#20065 = ORIENTED_EDGE ( 'NONE', *, *, #14116, .F. ) ;
#20066 = EDGE_CURVE ( 'NONE', #18527, #20316, #23398, .T. ) ;
#20067 = EDGE_LOOP ( 'NONE', ( #20843, #16721, #20563, #15753, #4360, #20112 ) ) ;
#20068 = VERTEX_POINT ( 'NONE', #18666 ) ;
#20069 = CARTESIAN_POINT ( 'NONE',  ( 87.67068093254673045, 7.562528597612068045E-15, 0.000000000000000000 ) ) ;
#20070 = EDGE_CURVE ( 'NONE', #21243, #10046, #8952, .T. ) ;
#20071 = AXIS2_PLACEMENT_3D ( 'NONE', #10932, #1824, #16570 ) ;
#20072 = DIRECTION ( 'NONE',  ( 0.000000000000000000, 0.000000000000000000, 1.000000000000000000 ) ) ;
#20073 = CARTESIAN_POINT ( 'NONE',  ( 0.000000000000000000, 0.000000000000000000, 11.00000000000000000 ) ) ;
#20074 = EDGE_LOOP ( 'NONE', ( #16790, #477, #22530, #1324 ) ) ;
#20075 = EDGE_CURVE ( 'NONE', #17414, #2739, #3522, .T. ) ;
#20076 = EDGE_CURVE ( 'NONE', #21535, #15398, #20022, .T. ) ;
#20077 = EDGE_CURVE ( 'NONE', #17518, #6728, #17530, .T. ) ;
#20078 = DIRECTION ( 'NONE',  ( 1.000000000000000000, 1.224606353822377258E-16, 0.000000000000000000 ) ) ;
#20079 = ORIENTED_EDGE ( 'NONE', *, *, #17791, .T. ) ;
#20080 = CYLINDRICAL_SURFACE ( 'NONE', #17267, 8.000000000000000000 ) ;
#20081 = CARTESIAN_POINT ( 'NONE',  ( 0.000000000000000000, 15.03999999999999737, 0.000000000000000000 ) ) ;
#20082 = DIRECTION ( 'NONE',  ( -1.000000000000000000, -0.000000000000000000, -0.000000000000000000 ) ) ;
#20083 = DIRECTION ( 'NONE',  ( -0.000000000000000000, -0.000000000000000000, -1.000000000000000000 ) ) ;
#20084 = VECTOR ( 'NONE', #19690, 1000.000000000000000 ) ;
#20085 = DIRECTION ( 'NONE',  ( 1.000000000000000000, 0.000000000000000000, 0.000000000000000000 ) ) ;
#20086 = CONICAL_SURFACE ( 'NONE', #4093, 5.024999999999998579, 0.7853981633974438381 ) ;
#20087 = LINE ( 'NONE', #21902, #7158 ) ;
#20088 = CARTESIAN_POINT ( 'NONE',  ( 3.136800900838523098E-15, 6.000000000000000000, 98.99999999999998579 ) ) ;
#20089 = CARTESIAN_POINT ( 'NONE',  ( -14.51962751333974211, 3.765689428759028790, -8.721787840009202597 ) ) ;
#20090 = CONICAL_SURFACE ( 'NONE', #271, 1.999999999999996669, 1.029744258676653867 ) ;
#20091 = CIRCLE ( 'NONE', #14239, 0.9999999999999991118 ) ;
#20092 = ORIENTED_EDGE ( 'NONE', *, *, #4485, .F. ) ;
#20093 = ADVANCED_BREP_SHAPE_REPRESENTATION ( '', ( #18256, #8005 ), #10756 ) ;
#20094 = CARTESIAN_POINT ( 'NONE',  ( 29.00000000000000000, 29.50000000000000000, -3.000000000000000000 ) ) ;
#20095 = PRESENTATION_LAYER_ASSIGNMENT (  '', '', ( #601 ) ) ;
#20096 = ORIENTED_EDGE ( 'NONE', *, *, #16676, .F. ) ;
#20097 = EDGE_CURVE ( 'NONE', #21933, #15211, #10893, .T. ) ;
#20098 = FACE_OUTER_BOUND ( 'NONE', #8690, .T. ) ;
#20099 = EDGE_LOOP ( 'NONE', ( #6239, #5883, #19798, #18064 ) ) ;
#20100 = ORIENTED_EDGE ( 'NONE', *, *, #21263, .F. ) ;
#20101 = APPLICATION_CONTEXT ( 'automotive_design' ) ;
#20102 = CARTESIAN_POINT ( 'NONE',  ( -9.388305250079428177, 0.5130848116249094870, -12.11169474992057005 ) ) ;
#20103 = CARTESIAN_POINT ( 'NONE',  ( 7.685661446562381371, -5.583959896777971110, -3.859589141758143604 ) ) ;
#20104 = VECTOR ( 'NONE', #20714, 1000.000000000000000 ) ;
#20105 = VECTOR ( 'NONE', #10961, 1000.000000000000000 ) ;
#20106 = DIRECTION ( 'NONE',  ( -0.5735764363510519326, 0.8191520442889876907, 1.003171929053519816E-16 ) ) ;
#20107 = DIRECTION ( 'NONE',  ( -1.000000000000000000, 0.000000000000000000, 0.000000000000000000 ) ) ;
#20108 = DIRECTION ( 'NONE',  ( -1.000000000000000000, 0.000000000000000000, 0.000000000000000000 ) ) ;
#20110 = ADVANCED_FACE ( 'NONE', ( #7195 ), #21969, .F. ) ;
#20109 = CIRCLE ( 'NONE', #4532, 7.999999999999992895 ) ;
#20111 = CARTESIAN_POINT ( 'NONE',  ( -9.500000000000000000, -6.482511860946779655E-13, 7.059589141758143782 ) ) ;
#20112 = ORIENTED_EDGE ( 'NONE', *, *, #7197, .F. ) ;
#20113 = CIRCLE ( 'NONE', #18557, 6.050000000006050094 ) ;
#20114 = CARTESIAN_POINT ( 'NONE',  ( -36.00000000000000711, -51.00000000000000711, 0.5000000000000000000 ) ) ;
#20115 = DIRECTION ( 'NONE',  ( 0.000000000000000000, 0.000000000000000000, -1.000000000000000000 ) ) ;
#20116 = DIRECTION ( 'NONE',  ( 0.4828336235133057208, -0.8757121056631633760, 0.000000000000000000 ) ) ;
#20117 = FACE_OUTER_BOUND ( 'NONE', #11377, .T. ) ;
#20118 = CARTESIAN_POINT ( 'NONE',  ( 17.49066032632880763, 9.200828712690864108, 2.414248458042549839 ) ) ;
#20119 = CARTESIAN_POINT ( 'NONE',  ( -31.74999999999995737, 0.000000000000000000, 0.000000000000000000 ) ) ;
#20120 = VERTEX_POINT ( 'NONE', #12682 ) ;
#20121 = DIRECTION ( 'NONE',  ( 0.000000000000000000, 0.000000000000000000, 1.000000000000000000 ) ) ;
#20122 = VECTOR ( 'NONE', #4342, 1000.000000000000114 ) ;
#20123 = DIRECTION ( 'NONE',  ( 0.000000000000000000, 0.000000000000000000, 1.000000000000000000 ) ) ;
#20124 = EDGE_LOOP ( 'NONE', ( #11030, #5033, #12824, #1594, #5684, #1673, #20500, #3963, #20144, #5873 ) ) ;
#20125 = TOROIDAL_SURFACE ( 'NONE', #10742, 21.85000000000000142, 1.000000000000000000 ) ;
#20126 = ORIENTED_EDGE ( 'NONE', *, *, #20724, .T. ) ;
#20127 = CARTESIAN_POINT ( 'NONE',  ( 7.685661446562381371, -5.583959896777971110, 9.006742014460233037 ) ) ;
#20128 = CARTESIAN_POINT ( 'NONE',  ( -6.822232771736903637E-13, 9.988891130263535700, 9.706742014460232326 ) ) ;
#20129 = CARTESIAN_POINT ( 'NONE',  ( 0.000000000000000000, -15.03999999999999915, 25.00000000000000000 ) ) ;
#20130 = ORIENTED_EDGE ( 'NONE', *, *, #17361, .F. ) ;
#20131 = VERTEX_POINT ( 'NONE', #7414 ) ;
#20132 = DIRECTION ( 'NONE',  ( 1.000000000000000000, 0.000000000000000000, 0.000000000000000000 ) ) ;
#20133 = LINE ( 'NONE', #8633, #9767 ) ;
#20134 = DIRECTION ( 'NONE',  ( -0.4011779117250717785, 0.9160001545545232160, 0.000000000000000000 ) ) ;
#20135 = ADVANCED_FACE ( 'NONE', ( #22213 ), #3304, .F. ) ;
#20136 = CARTESIAN_POINT ( 'NONE',  ( 23.00000000000000000, 0.000000000000000000, 0.000000000000000000 ) ) ;
#20137 = CARTESIAN_POINT ( 'NONE',  ( 40.89823313241237912, 26.41789760203348081, -27.00000000000000000 ) ) ;
#20138 = DIRECTION ( 'NONE',  ( 0.5000000000000001110, -0.8660254037844384856, 0.000000000000000000 ) ) ;
#20139 = CARTESIAN_POINT ( 'NONE',  ( 27.70933665152130132, 40.41277845351218190, 12.00000000000000000 ) ) ;
#20140 = CIRCLE ( 'NONE', #266, 5.000000000000007994 ) ;
#20141 = EDGE_CURVE ( 'NONE', #9278, #12486, #22331, .T. ) ;
#20142 = AXIS2_PLACEMENT_3D ( 'NONE', #15564, #13516, #4619 ) ;
#20143 = CARTESIAN_POINT ( 'NONE',  ( -2.935661446562617183, 9.035036904803758873, -10.65958914175814343 ) ) ;
#20144 = ORIENTED_EDGE ( 'NONE', *, *, #19881, .F. ) ;
#20145 = CIRCLE ( 'NONE', #18966, 1.999999999999997113 ) ;
#20146 = VERTEX_POINT ( 'NONE', #14639 ) ;
#20147 = FACE_OUTER_BOUND ( 'NONE', #15036, .T. ) ;
#20148 = CARTESIAN_POINT ( 'NONE',  ( -9.500000000000220268, 3.086737114211950406, 10.95958914175814236 ) ) ;
#20149 = CARTESIAN_POINT ( 'NONE',  ( 42.00000000000000000, -5.000000000000016875, 8.500000000000000000 ) ) ;
#20150 = CARTESIAN_POINT ( 'NONE',  ( -2.935661446561384391, -9.035036904804158553, -11.45958914175814414 ) ) ;
#20151 = DIRECTION ( 'NONE',  ( -1.000000000000000000, 0.000000000000000000, 0.000000000000000000 ) ) ;
#20152 = DIRECTION ( 'NONE',  ( -0.8757121056631640421, 0.4828336235133042775, 0.000000000000000000 ) ) ;
#20153 = ORIENTED_EDGE ( 'NONE', *, *, #3538, .T. ) ;
#20154 = DIRECTION ( 'NONE',  ( 1.000000000000000000, 0.000000000000000000, 0.000000000000000000 ) ) ;
#20155 = ORIENTED_EDGE ( 'NONE', *, *, #5248, .F. ) ;
#20156 = DIRECTION ( 'NONE',  ( 0.8757121056631640421, -0.4828336235133042775, 0.000000000000000000 ) ) ;
#20157 = DIRECTION ( 'NONE',  ( 0.000000000000000000, -1.000000000000000000, 0.000000000000000000 ) ) ;
#20158 = ADVANCED_FACE ( 'NONE', ( #12911 ), #15174, .T. ) ;
#20159 = VECTOR ( 'NONE', #20380, 1000.000000000000000 ) ;
#20160 = ORIENTED_EDGE ( 'NONE', *, *, #8637, .F. ) ;
#20161 = CARTESIAN_POINT ( 'NONE',  ( 7.937578510445243651, -3.514536757623948127, -12.49999999999998046 ) ) ;
#20162 = EDGE_LOOP ( 'NONE', ( #536, #16296, #7360, #2403, #13161 ) ) ;
#20163 = CARTESIAN_POINT ( 'NONE',  ( 23.00000000000000000, -8.772759796005278332, 7.720943453482002283 ) ) ;
#20164 = EDGE_CURVE ( 'NONE', #3028, #5633, #18552, .T. ) ;
#20165 = CARTESIAN_POINT ( 'NONE',  ( 0.000000000000000000, 15.50000000000000000, 16.70000000000000284 ) ) ;
#20166 = VERTEX_POINT ( 'NONE', #8900 ) ;
#20167 = DIRECTION ( 'NONE',  ( 0.000000000000000000, -1.224646799147353207E-16, 1.000000000000000000 ) ) ;
#20168 = LINE ( 'NONE', #3998, #1018 ) ;
#20169 = CARTESIAN_POINT ( 'NONE',  ( -6.822232771736903637E-13, 9.988891130263535700, -5.706742014460234103 ) ) ;
#20170 = ORIENTED_EDGE ( 'NONE', *, *, #22149, .F. ) ;
#20171 = CARTESIAN_POINT ( 'NONE',  ( -34.00000000000000000, 4.999999999999999112, 9.500000000000000000 ) ) ;
#20172 = DIRECTION ( 'NONE',  ( -1.000000000000000000, -0.000000000000000000, -0.000000000000000000 ) ) ;
#20173 = SURFACE_STYLE_FILL_AREA ( #5401 ) ;
#20174 = VERTEX_POINT ( 'NONE', #1835 ) ;
#20175 = CARTESIAN_POINT ( 'NONE',  ( 85.05659179472598908, -9.244463733058732095E-30, 5.000000000000007994 ) ) ;
#20176 = CARTESIAN_POINT ( 'NONE',  ( 15.00000000000000000, 6.781880092842756171E-15, 9.499999999999987566 ) ) ;
#20177 = CARTESIAN_POINT ( 'NONE',  ( 30.16774287754691386, -40.66994976491903913, -1.500000000000000000 ) ) ;
#20178 = EDGE_LOOP ( 'NONE', ( #15413, #2726, #17297, #15748 ) ) ;
#20179 = CARTESIAN_POINT ( 'NONE',  ( 2.935661446561383503, 9.035036904804158553, -9.606742014460232681 ) ) ;
#20180 = LINE ( 'NONE', #14189, #20744 ) ;
#20181 = CARTESIAN_POINT ( 'NONE',  ( 0.000000000000000000, 0.000000000000000000, 12.50000000000000000 ) ) ;
#20182 = EDGE_CURVE ( 'NONE', #1507, #9181, #22605, .T. ) ;
#20183 = DIRECTION ( 'NONE',  ( -1.000000000000000000, 0.000000000000000000, 0.000000000000000000 ) ) ;
#20184 = EDGE_CURVE ( 'NONE', #21416, #16900, #5377, .T. ) ;
#20185 = EDGE_CURVE ( 'NONE', #15133, #12561, #11070, .T. ) ;
#20186 = CIRCLE ( 'NONE', #20965, 8.000000000000000000 ) ;
#20187 = ORIENTED_EDGE ( 'NONE', *, *, #20204, .F. ) ;
#20188 = ORIENTED_EDGE ( 'NONE', *, *, #20208, .T. ) ;
#20189 = CARTESIAN_POINT ( 'NONE',  ( 40.89823313241238623, -26.41789760203348081, -27.00000000000000000 ) ) ;
#20190 = DIRECTION ( 'NONE',  ( -1.000000000000000000, 0.000000000000000000, 0.000000000000000000 ) ) ;
#20191 = ORIENTED_EDGE ( 'NONE', *, *, #6468, .F. ) ;
#20192 = ORIENTED_EDGE ( 'NONE', *, *, #11612, .F. ) ;
#20193 = DIRECTION ( 'NONE',  ( 0.000000000000000000, -1.000000000000000000, 0.000000000000000000 ) ) ;
#20194 = VERTEX_POINT ( 'NONE', #11187 ) ;
#20195 = DIRECTION ( 'NONE',  ( -1.000000000000000000, 0.000000000000000000, 0.000000000000000000 ) ) ;
#20196 = DIRECTION ( 'NONE',  ( -0.5735764363510519326, 0.8191520442889876907, 1.003171929053519816E-16 ) ) ;
#20197 = DIRECTION ( 'NONE',  ( -1.000000000000000000, -1.224606353822377258E-16, -0.000000000000000000 ) ) ;
#20198 = FACE_OUTER_BOUND ( 'NONE', #19770, .T. ) ;
#20199 = CARTESIAN_POINT ( 'NONE',  ( -40.77574956473004164, 27.49633847812775755, 11.00000000000000000 ) ) ;
#20200 = PRODUCT_RELATED_PRODUCT_CATEGORY ( 'part', '', ( #9355 ) ) ;
#20201 = AXIS2_PLACEMENT_3D ( 'NONE', #5923, #17263, #4108 ) ;
#20202 = CARTESIAN_POINT ( 'NONE',  ( 15.07341617659253963, -4.495283618570416806, 8.379779594489201955 ) ) ;
#20203=STYLED_ITEM('',(#24162),#2159);
#20204 = EDGE_CURVE ( 'NONE', #20932, #20166, #16236, .T. ) ;
#20205 = DIRECTION ( 'NONE',  ( -0.000000000000000000, -0.000000000000000000, 1.000000000000000000 ) ) ;
#20206 = CYLINDRICAL_SURFACE ( 'NONE', #23510, 4.999999999999997335 ) ;
#20207 = CARTESIAN_POINT ( 'NONE',  ( 27.89784171216407316, -41.49349862090490149, -1.500000000000000000 ) ) ;
#20208 = EDGE_CURVE ( 'NONE', #15969, #13092, #23410, .T. ) ;
#20209 = EDGE_LOOP ( 'NONE', ( #9272, #16692, #21638, #3551 ) ) ;
#20210 = CARTESIAN_POINT ( 'NONE',  ( 7.022953521755574080, -5.102474405759714671, 8.433165578109187877 ) ) ;
#20211 = ORIENTED_EDGE ( 'NONE', *, *, #11342, .F. ) ;
#20212 = EDGE_CURVE ( 'NONE', #20510, #12845, #5485, .T. ) ;
#20213 = AXIS2_PLACEMENT_3D ( 'NONE', #12953, #22373, #1868 ) ;
#20214 = EDGE_CURVE ( 'NONE', #21150, #2165, #15205, .T. ) ;
#20215 = APPLICATION_PROTOCOL_DEFINITION ( 'draft international standard', 'automotive_design', 1998, #2636 ) ;
#20216 = CARTESIAN_POINT ( 'NONE',  ( 0.000000000000000000, 0.000000000000000000, 0.4999999999999995559 ) ) ;
#20217 = EDGE_LOOP ( 'NONE', ( #22291, #9855, #18019, #5059, #15060 ) ) ;
#20218 = ORIENTED_EDGE ( 'NONE', *, *, #20814, .T. ) ;
#20219 = CARTESIAN_POINT ( 'NONE',  ( 60.90909090909091361, -4.172000000000000597, 0.000000000000000000 ) ) ;
#20220 = CARTESIAN_POINT ( 'NONE',  ( -7.685661446562381371, 5.583959896777970222, -8.859589141758144493 ) ) ;
#20221 = FACE_OUTER_BOUND ( 'NONE', #17497, .T. ) ;
#20222 = CARTESIAN_POINT ( 'NONE',  ( 5.000000000000000000, -2.342598717236905603, 4.057500000000010765 ) ) ;
#20223 = CARTESIAN_POINT ( 'NONE',  ( 76.03431729618309021, 7.562528597612068045E-15, 0.000000000000000000 ) ) ;
#20224 = ORIENTED_EDGE ( 'NONE', *, *, #11528, .F. ) ;
#20225 = CARTESIAN_POINT ( 'NONE',  ( 23.85000000000000142, -15.03999999999999737, 2.200000000000000178 ) ) ;
#20226 = ORIENTED_EDGE ( 'NONE', *, *, #18852, .F. ) ;
#20227 = CARTESIAN_POINT ( 'NONE',  ( 20.85000000000000853, 15.03999999999999915, 25.00000000000000000 ) ) ;
#20228 = DIRECTION ( 'NONE',  ( -1.000000000000000000, -1.224606353822377258E-16, -0.000000000000000000 ) ) ;
#20229 = CARTESIAN_POINT ( 'NONE',  ( 23.00000000000000000, -15.26463740537730907, 9.300885435430052084 ) ) ;
#20230 = CARTESIAN_POINT ( 'NONE',  ( 17.59008829125738416, 9.499485695642613692, 0.4958780962348190990 ) ) ;
#20231 = ADVANCED_FACE ( 'NONE', ( #11671 ), #15471, .T. ) ;
#20232 = DIRECTION ( 'NONE',  ( -1.000000000000000000, 0.000000000000000000, 0.000000000000000000 ) ) ;
#20233 = CARTESIAN_POINT ( 'NONE',  ( 78.36363636363637397, 4.172000000000015696, 0.000000000000000000 ) ) ;
#20234 = CARTESIAN_POINT ( 'NONE',  ( 2.935661446562616295, -9.035036904803758873, -10.80674201446023197 ) ) ;
#20235 = CARTESIAN_POINT ( 'NONE',  ( 3.890962118697714531E-15, 15.50000000000000000, 19.70000000000000284 ) ) ;
#20236 = VERTEX_POINT ( 'NONE', #19272 ) ;
#20237 = ORIENTED_EDGE ( 'NONE', *, *, #2738, .F. ) ;
#20238 =( REPRESENTATION_RELATIONSHIP ('NONE','NONE', #21748, #8762 ) REPRESENTATION_RELATIONSHIP_WITH_TRANSFORMATION ( #9427 )SHAPE_REPRESENTATION_RELATIONSHIP( ) );
#20239 = CARTESIAN_POINT ( 'NONE',  ( 9.499999999999790390, 3.086737114213260025, 9.306742014460233747 ) ) ;
#20240 = CARTESIAN_POINT ( 'NONE',  ( 2.935661446561383503, 9.035036904804158553, 5.606742014460233570 ) ) ;
#20241 = ADVANCED_FACE ( 'NONE', ( #17058 ), #9354, .T. ) ;
#20242 = EDGE_LOOP ( 'NONE', ( #52, #20707, #20275, #7967 ) ) ;
#20243 = EDGE_CURVE ( 'NONE', #1485, #19491, #125, .T. ) ;
#20244 = ORIENTED_EDGE ( 'NONE', *, *, #14548, .F. ) ;
#20245 = CARTESIAN_POINT ( 'NONE',  ( 0.000000000000000000, 0.000000000000000000, 0.000000000000000000 ) ) ;
#20246 = CARTESIAN_POINT ( 'NONE',  ( 67.60204634018053582, -5.000000000000009770, 0.000000000000000000 ) ) ;
#20247 = CARTESIAN_POINT ( 'NONE',  ( -9.499999999999790390, -3.086737114213257804, -4.306742014460233747 ) ) ;
#20248 = CARTESIAN_POINT ( 'NONE',  ( 0.000000000000000000, 0.000000000000000000, 0.000000000000000000 ) ) ;
#20249 = PRESENTATION_STYLE_ASSIGNMENT (( #13259 ) ) ;
#20250 = DIRECTION ( 'NONE',  ( -1.000000000000000000, -1.224606353822377258E-16, -0.000000000000000000 ) ) ;
#20251 = ORIENTED_EDGE ( 'NONE', *, *, #2815, .T. ) ;
#20252 = VERTEX_POINT ( 'NONE', #20728 ) ;
#20253 = DIRECTION ( 'NONE',  ( -0.000000000000000000, -0.000000000000000000, -1.000000000000000000 ) ) ;
#20254 = ORIENTED_EDGE ( 'NONE', *, *, #2880, .T. ) ;
#20255 = LINE ( 'NONE', #23793, #1988 ) ;
#20256 = FACE_OUTER_BOUND ( 'NONE', #10081, .T. ) ;
#20257 = DIRECTION ( 'NONE',  ( 0.000000000000000000, -1.000000000000000000, 0.000000000000000000 ) ) ;
#20258 = CARTESIAN_POINT ( 'NONE',  ( 0.000000000000000000, -15.26463740537718827, -9.300885435430258141 ) ) ;
#20259 = DIRECTION ( 'NONE',  ( -0.000000000000000000, -0.000000000000000000, -1.000000000000000000 ) ) ;
#20260 = CIRCLE ( 'NONE', #23347, 11.68650000001168721 ) ;
#20261 = CARTESIAN_POINT ( 'NONE',  ( 2.024999999999999911, -45.00000000000000000, 27.00000000000000000 ) ) ;
#20262 = ORIENTED_EDGE ( 'NONE', *, *, #15829, .F. ) ;
#20263 = DIRECTION ( 'NONE',  ( -1.000000000000000000, 0.000000000000000000, 0.000000000000000000 ) ) ;
#20264 = ORIENTED_EDGE ( 'NONE', *, *, #15232, .T. ) ;
#20265 = AXIS2_PLACEMENT_3D ( 'NONE', #18801, #15233, #5995 ) ;
#20266 = DIRECTION ( 'NONE',  ( -0.000000000000000000, -0.000000000000000000, -1.000000000000000000 ) ) ;
#20267 = EDGE_CURVE ( 'NONE', #4656, #22118, #18770, .T. ) ;
#20268 = ORIENTED_EDGE ( 'NONE', *, *, #1289, .F. ) ;
#20269 = CARTESIAN_POINT ( 'NONE',  ( 43.49999999999997868, -25.84341543330623381, 0.000000000000000000 ) ) ;
#20270 = CARTESIAN_POINT ( 'NONE',  ( 65.85249911436491743, 5.000000000000015987, 0.000000000000000000 ) ) ;
#20271 = CARTESIAN_POINT ( 'NONE',  ( -2.352265130537804616, -9.224593858589891227, -3.479461880036829768 ) ) ;
#20272 = DIRECTION ( 'NONE',  ( -0.000000000000000000, -0.000000000000000000, 1.000000000000000000 ) ) ;
#20273 = DIRECTION ( 'NONE',  ( -1.000000000000000000, 0.000000000000000000, 0.000000000000000000 ) ) ;
#20274 = CARTESIAN_POINT ( 'NONE',  ( -7.685661446561619314, -5.583959896779019161, -5.259589141758143960 ) ) ;
#20275 = ORIENTED_EDGE ( 'NONE', *, *, #24079, .T. ) ;
#20276 = VERTEX_POINT ( 'NONE', #22561 ) ;
#20277 = LINE ( 'NONE', #16485, #4874 ) ;
#20278 = VECTOR ( 'NONE', #23798, 1000.000000000000000 ) ;
#20279 = FACE_OUTER_BOUND ( 'NONE', #17509, .T. ) ;
#20280 = EDGE_CURVE ( 'NONE', #15584, #5444, #5223, .T. ) ;
#20281 = CARTESIAN_POINT ( 'NONE',  ( 35.99999999999999289, 50.99999999999999289, 12.50000000000000000 ) ) ;
#20282 = EDGE_CURVE ( 'NONE', #4922, #7241, #20614, .T. ) ;
#20283 = VERTEX_POINT ( 'NONE', #9481 ) ;
#20284 = LINE ( 'NONE', #7099, #10613 ) ;
#20285 = CYLINDRICAL_SURFACE ( 'NONE', #14165, 15.00000000000000000 ) ;
#20286 = ORIENTED_EDGE ( 'NONE', *, *, #8172, .T. ) ;
#20287 = DIRECTION ( 'NONE',  ( -0.000000000000000000, -0.000000000000000000, -1.000000000000000000 ) ) ;
#20288 = EDGE_CURVE ( 'NONE', #8991, #13594, #16940, .T. ) ;
#20289 = DIRECTION ( 'NONE',  ( -1.000000000000000000, -0.000000000000000000, -0.000000000000000000 ) ) ;
#20290 = FACE_OUTER_BOUND ( 'NONE', #2928, .T. ) ;
#20291 = CARTESIAN_POINT ( 'NONE',  ( 2.682529543900284974, -8.255977015246234174, 6.233165578109188587 ) ) ;
#20292 = CIRCLE ( 'NONE', #808, 1.500000000000001332 ) ;
#20293 = ORIENTED_EDGE ( 'NONE', *, *, #18660, .T. ) ;
#20294 = ORIENTED_EDGE ( 'NONE', *, *, #16916, .F. ) ;
#20295 = ORIENTED_EDGE ( 'NONE', *, *, #14086, .F. ) ;
#20296 = EDGE_LOOP ( 'NONE', ( #5863, #14881, #3789, #15982 ) ) ;
#20297 = CYLINDRICAL_SURFACE ( 'NONE', #20866, 5.000000000000000888 ) ;
#20298 = CARTESIAN_POINT ( 'NONE',  ( 33.99999999999998579, 5.999999999999985789, 12.00000000000000000 ) ) ;
#20299 = ORIENTED_EDGE ( 'NONE', *, *, #15159, .F. ) ;
#20300 = ORIENTED_EDGE ( 'NONE', *, *, #4493, .F. ) ;
#20301 = ADVANCED_FACE ( 'NONE', ( #2306 ), #4152, .F. ) ;
#20302 = DIRECTION ( 'NONE',  ( -0.000000000000000000, -0.000000000000000000, -1.000000000000000000 ) ) ;
#20303 = ORIENTED_EDGE ( 'NONE', *, *, #10998, .T. ) ;
#20304 =( BOUNDED_CURVE ( )  B_SPLINE_CURVE ( 2, ( #11180, #9475, #21961, #18658, #20143, #12903, #7187, #22207, #12794, #3650, #16932 ),
 .UNSPECIFIED., .F., .F. ) 
 B_SPLINE_CURVE_WITH_KNOTS ( ( 3, 2, 2, 2, 2, 3 ),
 ( 0.09999999999999992228, 0.1199999999999999262, 0.1399999999999999578, 0.1599999999999999756, 0.1799999999999999656, 0.2000000000000000111 ),
 .UNSPECIFIED. ) 
 CURVE ( )  GEOMETRIC_REPRESENTATION_ITEM ( )  RATIONAL_B_SPLINE_CURVE ( ( 1.000000000000000222, 0.9510565162951533091, 1.000000000000000000, 0.9510565162951535312, 1.000000000000000000, 0.9510565162951535312, 1.000000000000000000, 0.9510565162951535312, 1.000000000000000000, 0.9510565162951535312, 1.000000000000000000 ) ) 
 REPRESENTATION_ITEM ( '' )  );
#20305 = AXIS2_PLACEMENT_3D ( 'NONE', #7290, #19996, #12523 ) ;
#20306 = EDGE_CURVE ( 'NONE', #3333, #10964, #554, .T. ) ;
#20307 = ADVANCED_FACE ( 'NONE', ( #359 ), #15342, .T. ) ;
#20308 = FACE_OUTER_BOUND ( 'NONE', #20178, .T. ) ;
#20309 = FACE_OUTER_BOUND ( 'NONE', #2799, .T. ) ;
#20310 = FACE_BOUND ( 'NONE', #4808, .T. ) ;
#20311 = AXIS2_PLACEMENT_3D ( 'NONE', #23879, #11040, #20464 ) ;
#20312 = CARTESIAN_POINT ( 'NONE',  ( 87.96568270381690979, 6.123233995736675563E-16, -5.000000000000007994 ) ) ;
#20313 = CARTESIAN_POINT ( 'NONE',  ( -6.249999999999999112, -10.82531754730548279, 2.500000000000000000 ) ) ;
#20314 = DIRECTION ( 'NONE',  ( 0.000000000000000000, -1.000000000000000000, 0.000000000000000000 ) ) ;
#20315 = LINE ( 'NONE', #16752, #6081 ) ;
#20316 = VERTEX_POINT ( 'NONE', #22814 ) ;
#20317 = CARTESIAN_POINT ( 'NONE',  ( -8.680847955710813579, -2.820578480814258437, 7.733165578109187699 ) ) ;
#20318 = VERTEX_POINT ( 'NONE', #13535 ) ;
#20319 = APPLICATION_PROTOCOL_DEFINITION ( 'draft international standard', 'automotive_design', 1998, #5736 ) ;
#20320 = DIRECTION ( 'NONE',  ( 0.000000000000000000, 0.000000000000000000, 1.000000000000000000 ) ) ;
#20321 = CIRCLE ( 'NONE', #19157, 5.000000000000007994 ) ;
#20322 = ORIENTED_EDGE ( 'NONE', *, *, #23513, .F. ) ;
#20323 = ORIENTED_EDGE ( 'NONE', *, *, #4708, .T. ) ;
#20324 = CARTESIAN_POINT ( 'NONE',  ( -30.32370777929697425, -42.16181938034195298, -1.500000000000000000 ) ) ;
#20325 = CARTESIAN_POINT ( 'NONE',  ( 5.365059087798938364, 7.384370330707087149, -8.933165578109186100 ) ) ;
#20326 = AXIS2_PLACEMENT_3D ( 'NONE', #7592, #18969, #2242 ) ;
#20327 = ORIENTED_EDGE ( 'NONE', *, *, #20584, .F. ) ;
#20328 = DIRECTION ( 'NONE',  ( -1.000000000000000000, -1.224606353822377258E-16, -0.000000000000000000 ) ) ;
#20329 = CARTESIAN_POINT ( 'NONE',  ( 11.50000000000000000, 17.26667456984545268, -4.623588898214372023 ) ) ;
#20330 = CARTESIAN_POINT ( 'NONE',  ( -20.99999999999999645, 29.49999999999999645, 11.50000000000000000 ) ) ;
#20331 = DIRECTION ( 'NONE',  ( -1.000000000000000000, 0.000000000000000000, 0.000000000000000000 ) ) ;
#20332 = EDGE_LOOP ( 'NONE', ( #21734, #14480, #9701, #16479, #21258 ) ) ;
#20333 = DIRECTION ( 'NONE',  ( -1.000000000000000000, -1.337728473353585242E-16, 0.000000000000000000 ) ) ;
#20334 = ORIENTED_EDGE ( 'NONE', *, *, #22363, .T. ) ;
#20335 = EDGE_CURVE ( 'NONE', #14903, #21740, #4268, .T. ) ;
#20336 = EDGE_CURVE ( 'NONE', #11923, #23352, #2789, .T. ) ;
#20337 = ORIENTED_EDGE ( 'NONE', *, *, #7913, .F. ) ;
#20338 = CARTESIAN_POINT ( 'NONE',  ( 20.64923905428957340, 37.45138642374540439, 12.00000000000000000 ) ) ;
#20339 = LINE ( 'NONE', #18517, #17581 ) ;
#20340 = DIRECTION ( 'NONE',  ( 0.7052211081716891483, 0.7089874389501515939, -0.000000000000000000 ) ) ;
#20341 = SURFACE_STYLE_FILL_AREA ( #23883 ) ;
#20342 = CONICAL_SURFACE ( 'NONE', #15654, 5.000000000000007994, 0.9599310885968855844 ) ;
#20343 = CYLINDRICAL_SURFACE ( 'NONE', #4861, 5.000000000000000888 ) ;
#20344 = LINE ( 'NONE', #3151, #11374 ) ;
#20345 = CARTESIAN_POINT ( 'NONE',  ( -9.500000000000000000, -6.482511860946779655E-13, -10.20674201446023233 ) ) ;
#20346 = DIRECTION ( 'NONE',  ( -1.000000000000000000, -0.000000000000000000, -0.000000000000000000 ) ) ;
#20347 = EDGE_LOOP ( 'NONE', ( #19582, #3679, #17027, #17259 ) ) ;
#20348 = ORIENTED_EDGE ( 'NONE', *, *, #3511, .F. ) ;
#20349 = CARTESIAN_POINT ( 'NONE',  ( 9.499999999999790390, 3.086737114213260025, 7.306742014460234635 ) ) ;
#20350 = CARTESIAN_POINT ( 'NONE',  ( -5.871322893124554021, 8.081182679343978492, 3.906742014460231616 ) ) ;
#20351 = EDGE_LOOP ( 'NONE', ( #18382, #10038, #14615, #18982, #9616 ) ) ;
#20352 = VERTEX_POINT ( 'NONE', #15850 ) ;
#20353 = CARTESIAN_POINT ( 'NONE',  ( -9.000000000000000000, 0.000000000000000000, 53.00000000000000000 ) ) ;
#20354 = EDGE_CURVE ( 'NONE', #23418, #21066, #14560, .T. ) ;
#20355 = CARTESIAN_POINT ( 'NONE',  ( 30.44534269664589843, 40.40463133211081015, 27.00000000000000000 ) ) ;
#20356 = AXIS2_PLACEMENT_3D ( 'NONE', #4142, #11557, #11665 ) ;
#20357 = CARTESIAN_POINT ( 'NONE',  ( 28.99999999999998579, -29.49999999999999645, -1.500000000000000000 ) ) ;
#20358 = AXIS2_PLACEMENT_3D ( 'NONE', #9390, #15247, #15019 ) ;
#20359 = AXIS2_PLACEMENT_3D ( 'NONE', #1097, #10694, #1461 ) ;
#20360 = CIRCLE ( 'NONE', #6340, 1.000000000000000888 ) ;
#20361 = CIRCLE ( 'NONE', #12183, 5.000000000000007994 ) ;
#20362 = CARTESIAN_POINT ( 'NONE',  ( 0.000000000000000000, 0.000000000000000000, 53.00000000000000000 ) ) ;
#20363 = VERTEX_POINT ( 'NONE', #15713 ) ;
#20364 = AXIS2_PLACEMENT_3D ( 'NONE', #18338, #16625, #24064 ) ;
#20365 = ADVANCED_FACE ( 'NONE', ( #19769 ), #21349, .T. ) ;
#20366 = EDGE_CURVE ( 'NONE', #12337, #12836, #22761, .T. ) ;
#20367 = PLANE ( 'NONE',  #13684 ) ;
#20368 = DIRECTION ( 'NONE',  ( 0.000000000000000000, 0.000000000000000000, 1.000000000000000000 ) ) ;
#20369 = AXIS2_PLACEMENT_3D ( 'NONE', #21864, #4472, #16356 ) ;
#20370 = CARTESIAN_POINT ( 'NONE',  ( -17.19784311473120653, 8.411123426659422364, -4.422670359120419725 ) ) ;
#20371 = DIRECTION ( 'NONE',  ( 0.000000000000000000, 0.000000000000000000, 1.000000000000000000 ) ) ;
#20372 = DIRECTION ( 'NONE',  ( 5.501724186093585079E-16, 1.000000000000000000, -0.000000000000000000 ) ) ;
#20373 = ORIENTED_EDGE ( 'NONE', *, *, #5084, .F. ) ;
#20374 = ORIENTED_EDGE ( 'NONE', *, *, #11115, .F. ) ;
#20375 = AXIS2_PLACEMENT_3D ( 'NONE', #16901, #214, #7626 ) ;
#20376 = LINE ( 'NONE', #1944, #9429 ) ;
#20377 = CIRCLE ( 'NONE', #6747, 2.000000000000000000 ) ;
#20378 = AXIS2_PLACEMENT_3D ( 'NONE', #22384, #16742, #24075 ) ;
#20379 = VERTEX_POINT ( 'NONE', #23541 ) ;
#20380 = DIRECTION ( 'NONE',  ( 0.000000000000000000, 1.000000000000000000, -0.000000000000000000 ) ) ;
#20381 = AXIS2_PLACEMENT_3D ( 'NONE', #22043, #19850, #10895 ) ;
#20382 = DIRECTION ( 'NONE',  ( 1.000000000000000000, 0.000000000000000000, 0.000000000000000000 ) ) ;
#20383 = AXIS2_PLACEMENT_3D ( 'NONE', #10953, #11802, #2677 ) ;
#20384 = CARTESIAN_POINT ( 'NONE',  ( -41.73082370883260239, 29.50000000000000711, -1.500000000000000000 ) ) ;
#20385 = EDGE_CURVE ( 'NONE', #4271, #21210, #16517, .T. ) ;
#20386 = CARTESIAN_POINT ( 'NONE',  ( -7.685661446561619314, -5.583959896779019161, -9.259589141758143072 ) ) ;
#20387 = EDGE_LOOP ( 'NONE', ( #12464, #8319 ) ) ;
#20388 = ORIENTED_EDGE ( 'NONE', *, *, #19811, .T. ) ;
#20389 = CARTESIAN_POINT ( 'NONE',  ( 69.05659179472598908, -9.244463733058732095E-30, 5.000000000000007994 ) ) ;
#20390 = AXIS2_PLACEMENT_3D ( 'NONE', #19233, #13733, #2516 ) ;
#20391 = VECTOR ( 'NONE', #17671, 1000.000000000000000 ) ;
#20392 = EDGE_CURVE ( 'NONE', #18951, #20194, #12228, .T. ) ;
#20393 = VERTEX_POINT ( 'NONE', #8396 ) ;
#20394 = DIRECTION ( 'NONE',  ( -1.000000000000000000, 0.000000000000000000, 0.000000000000000000 ) ) ;
#20395 = AXIS2_PLACEMENT_3D ( 'NONE', #20576, #16892, #13229 ) ;
#20396 = TOROIDAL_SURFACE ( 'NONE', #10630, 11.23654394515110511, 0.9599481167642566204 ) ;
#20397 = EDGE_LOOP ( 'NONE', ( #8105, #18762, #14516, #2700 ) ) ;
#20398 = AXIS2_PLACEMENT_3D ( 'NONE', #20248, #22447, #11287 ) ;
#20399 = CARTESIAN_POINT ( 'NONE',  ( 0.000000000000000000, 0.000000000000000000, 27.00000000000000000 ) ) ;
#20400 = FACE_OUTER_BOUND ( 'NONE', #11592, .T. ) ;
#20401 = DIRECTION ( 'NONE',  ( -0.000000000000000000, -0.000000000000000000, -1.000000000000000000 ) ) ;
#20402 = ORIENTED_EDGE ( 'NONE', *, *, #11084, .F. ) ;
#20403 = DIRECTION ( 'NONE',  ( 1.000000000000000000, 0.000000000000000000, -0.000000000000000000 ) ) ;
#20404 = FACE_OUTER_BOUND ( 'NONE', #15212, .T. ) ;
#20405 = CARTESIAN_POINT ( 'NONE',  ( 0.000000000000000000, 2.119223430970168742, 17.74893002550480858 ) ) ;
#20406 = CARTESIAN_POINT ( 'NONE',  ( -8.680847955710813579, -2.820578480814258437, 5.733165578109188587 ) ) ;
#20407 = ORIENTED_EDGE ( 'NONE', *, *, #17919, .F. ) ;
#20408 = ORIENTED_EDGE ( 'NONE', *, *, #10499, .F. ) ;
#20409 = ORIENTED_EDGE ( 'NONE', *, *, #13246, .T. ) ;
#20410 = CIRCLE ( 'NONE', #16510, 5.000000000000007994 ) ;
#20411 = CONTEXT_DEPENDENT_SHAPE_REPRESENTATION ( #22260, #17829 ) ;
#20412 = ADVANCED_FACE ( 'NONE', ( #12415 ), #2502, .F. ) ;
#20414 = ORIENTED_EDGE ( 'NONE', *, *, #6819, .T. ) ;
#20413 = VECTOR ( 'NONE', #6398, 999.9999999999998863 ) ;
#20415 = LINE ( 'NONE', #7454, #998 ) ;
#20416 = AXIS2_PLACEMENT_3D ( 'NONE', #17912, #3136, #8613 ) ;
#20417 = CYLINDRICAL_SURFACE ( 'NONE', #136, 10.00000000000000178 ) ;
#20418 = ORIENTED_EDGE ( 'NONE', *, *, #4550, .F. ) ;
#20419 = CIRCLE ( 'NONE', #21986, 5.000000000000007994 ) ;
#20420 = EDGE_CURVE ( 'NONE', #17607, #2619, #17672, .T. ) ;
#20421 = EDGE_CURVE ( 'NONE', #8401, #21516, #4054, .T. ) ;
#20422 = DIRECTION ( 'NONE',  ( 0.5735764363510424957, 0.8191520442889943521, 0.000000000000000000 ) ) ;
#20423 = ORIENTED_EDGE ( 'NONE', *, *, #21862, .F. ) ;
#20424 = DIRECTION ( 'NONE',  ( -0.000000000000000000, -0.000000000000000000, -1.000000000000000000 ) ) ;
#20425 = FACE_OUTER_BOUND ( 'NONE', #2210, .T. ) ;
#20426 = DIRECTION ( 'NONE',  ( -1.000000000000000000, 0.000000000000000000, 0.000000000000000000 ) ) ;
#20427 = FACE_OUTER_BOUND ( 'NONE', #6038, .T. ) ;
#20428 = VECTOR ( 'NONE', #3534, 1000.000000000000000 ) ;
#20429 = AXIS2_PLACEMENT_3D ( 'NONE', #2959, #8667, #6861 ) ;
#20430 = DIRECTION ( 'NONE',  ( -0.9913301211009815095, -0.1313947906041688374, 0.000000000000000000 ) ) ;
#20431 = LINE ( 'NONE', #13216, #6773 ) ;
#20432 = CARTESIAN_POINT ( 'NONE',  ( -10.83999999999999986, -14.99147757894464306, 0.000000000000000000 ) ) ;
#20433 = LINE ( 'NONE', #3482, #9956 ) ;
#20434 = CIRCLE ( 'NONE', #20833, 1.000000000000000888 ) ;
#20435 = ORIENTED_EDGE ( 'NONE', *, *, #8564, .T. ) ;
#20436 = CARTESIAN_POINT ( 'NONE',  ( -2.682529543900285862, 8.255977015246234174, 11.23316557810918859 ) ) ;
#20437 = EDGE_LOOP ( 'NONE', ( #4100, #11993, #12891, #1735, #16215, #6717, #15463, #20938, #17119, #19068, #10583, #11386, #18008, #19702 ) ) ;
#20438 = AXIS2_PLACEMENT_3D ( 'NONE', #1807, #16555, #5580 ) ;
#20439 = ADVANCED_FACE ( 'NONE', ( #1213 ), #6586, .T. ) ;
#20440 = SHAPE_DEFINITION_REPRESENTATION ( #15868, #12815 ) ;
#20441 = AXIS2_PLACEMENT_3D ( 'NONE', #22055, #7377, #22279 ) ;
#20442 = EDGE_LOOP ( 'NONE', ( #3799, #10500, #16484, #17371, #1292 ) ) ;
#20443 = VERTEX_POINT ( 'NONE', #21463 ) ;
#20444 = ADVANCED_FACE ( 'NONE', ( #4756 ), #19661, .F. ) ;
#20445 = FACE_OUTER_BOUND ( 'NONE', #13996, .T. ) ;
#20446 = CARTESIAN_POINT ( 'NONE',  ( -1.504652183083727168, 9.499999999999904077, -2.610843423304989308 ) ) ;
#20447 =( BOUNDED_CURVE ( )  B_SPLINE_CURVE ( 2, ( #9147, #23928, #133, #14990, #16595, #3543, #9488, #24044, #16949, #7665, #21979 ),
 .UNSPECIFIED., .F., .T. ) 
 B_SPLINE_CURVE_WITH_KNOTS ( ( 3, 2, 2, 2, 2, 3 ),
 ( 0.2000000000000000111, 0.2200000000000000289, 0.2400000000000000466, 0.2600000000000000644, 0.2800000000000001377, 0.3000000000000000999 ),
 .UNSPECIFIED. ) 
 CURVE ( )  GEOMETRIC_REPRESENTATION_ITEM ( )  RATIONAL_B_SPLINE_CURVE ( ( 1.000000000000000000, 0.9510565162951535312, 1.000000000000000000, 0.9510565162951535312, 1.000000000000000000, 0.9510565162951535312, 1.000000000000000000, 0.9510565162951535312, 1.000000000000000000, 0.9510565162951533091, 1.000000000000000222 ) ) 
 REPRESENTATION_ITEM ( '' )  );
#20448 = AXIS2_PLACEMENT_3D ( 'NONE', #20654, #9985, #11232 ) ;
#20449 = PLANE ( 'NONE',  #9468 ) ;
#20450 = EDGE_CURVE ( 'NONE', #1008, #21329, #9972, .T. ) ;
#20451 = VECTOR ( 'NONE', #12204, 1000.000000000000000 ) ;
#20452 = ORIENTED_EDGE ( 'NONE', *, *, #14977, .T. ) ;
#20453 = CARTESIAN_POINT ( 'NONE',  ( 23.00000000000000000, -13.61176534793449200, 4.089617900950054619 ) ) ;
#20454 = CARTESIAN_POINT ( 'NONE',  ( 0.000000000000000000, 15.23000000000000220, 27.00000000000000000 ) ) ;
#20455 = DIRECTION ( 'NONE',  ( -0.000000000000000000, -0.000000000000000000, -1.000000000000000000 ) ) ;
#20456 = CARTESIAN_POINT ( 'NONE',  ( 20.99999999999999645, -29.50000000000000355, 12.00000000000000000 ) ) ;
#20457 = AXIS2_PLACEMENT_3D ( 'NONE', #7632, #17275, #17034 ) ;
#20458 = DIRECTION ( 'NONE',  ( 4.613626265895764052E-16, -1.000000000000000000, 0.000000000000000000 ) ) ;
#20459 = DIRECTION ( 'NONE',  ( 1.337728473353585242E-16, -1.000000000000000000, 0.000000000000000000 ) ) ;
#20460 = ORIENTED_EDGE ( 'NONE', *, *, #1700, .F. ) ;
#20461 = CIRCLE ( 'NONE', #2540, 5.100000000000000533 ) ;
#20462 = ORIENTED_EDGE ( 'NONE', *, *, #247, .T. ) ;
#20463 = DIRECTION ( 'NONE',  ( -1.000000000000000000, -1.224606353822377258E-16, -0.000000000000000000 ) ) ;
#20464 = DIRECTION ( 'NONE',  ( 0.000000000000000000, -1.000000000000000000, 0.000000000000000000 ) ) ;
#20465 = CARTESIAN_POINT ( 'NONE',  ( 23.00000000000000000, 14.21257171757157245, 0.08908218613057176938 ) ) ;
#20466 = CARTESIAN_POINT ( 'NONE',  ( 20.85000000000000497, 15.03999999999999737, 2.200000000000000178 ) ) ;
#20467 = CONICAL_SURFACE ( 'NONE', #9924, 4.172000000000008590, 0.9599310885968742602 ) ;
#20468 = AXIS2_PLACEMENT_3D ( 'NONE', #596, #13391, #11784 ) ;
#20469 = LINE ( 'NONE', #11648, #3700 ) ;
#20470 = DIRECTION ( 'NONE',  ( -1.000000000000000000, -0.000000000000000000, -0.000000000000000000 ) ) ;
#20471 = DIRECTION ( 'NONE',  ( -0.000000000000000000, -0.000000000000000000, 1.000000000000000000 ) ) ;
#20472 = ORIENTED_EDGE ( 'NONE', *, *, #17728, .F. ) ;
#20473 = ORIENTED_EDGE ( 'NONE', *, *, #12704, .F. ) ;
#20474 = CARTESIAN_POINT ( 'NONE',  ( -5.871322893124554021, 8.081182679343978492, 11.90674201446023339 ) ) ;
#20475 = ORIENTED_EDGE ( 'NONE', *, *, #14447, .F. ) ;
#20476 = ORIENTED_EDGE ( 'NONE', *, *, #6310, .F. ) ;
#20477 = VECTOR ( 'NONE', #7941, 1000.000000000000000 ) ;
#20478 =( LENGTH_UNIT ( ) NAMED_UNIT ( * ) SI_UNIT ( .MILLI., .METRE. ) );
#20479 = VECTOR ( 'NONE', #19915, 1000.000000000000000 ) ;
#20480 = EDGE_LOOP ( 'NONE', ( #8503, #22442, #23231, #663 ) ) ;
#20481 = EDGE_CURVE ( 'NONE', #3315, #14363, #20419, .T. ) ;
#20482 = FACE_OUTER_BOUND ( 'NONE', #4666, .T. ) ;
#20483 = DIRECTION ( 'NONE',  ( 0.000000000000000000, 0.000000000000000000, 1.000000000000000000 ) ) ;
#20484 = EDGE_CURVE ( 'NONE', #20529, #18828, #9885, .T. ) ;
#20485 = CIRCLE ( 'NONE', #11881, 1.999999999999994449 ) ;
#20486 = CARTESIAN_POINT ( 'NONE',  ( -39.00000000000000000, -28.80990663662251805, 12.00000000000000000 ) ) ;
#20487 = DIRECTION ( 'NONE',  ( 0.000000000000000000, 0.000000000000000000, -1.000000000000000000 ) ) ;
#20488 = DIRECTION ( 'NONE',  ( -1.000000000000000000, -1.224606353822377258E-16, -0.000000000000000000 ) ) ;
#20489 = VERTEX_POINT ( 'NONE', #17808 ) ;
#20490 = LINE ( 'NONE', #3530, #15373 ) ;
#20491 = AXIS2_PLACEMENT_3D ( 'NONE', #2660, #17291, #10078 ) ;
#20492 = CARTESIAN_POINT ( 'NONE',  ( 9.500000000000000000, 6.470877716354879437E-13, 6.059589141758143782 ) ) ;
#20493 = CARTESIAN_POINT ( 'NONE',  ( -42.00000000000000000, -26.82133436441678853, 11.00000000000000000 ) ) ;
#20494 = CARTESIAN_POINT ( 'NONE',  ( -17.57831567727900790, 9.462949834988608089, 0.9681625741885162562 ) ) ;
#20495 = DIRECTION ( 'NONE',  ( 1.000000000000000000, 0.000000000000000000, 0.000000000000000000 ) ) ;
#20496 =( GEOMETRIC_REPRESENTATION_CONTEXT ( 3 ) GLOBAL_UNCERTAINTY_ASSIGNED_CONTEXT ( ( #8380 ) ) GLOBAL_UNIT_ASSIGNED_CONTEXT ( ( #7780, #9264, #22685 ) ) REPRESENTATION_CONTEXT ( 'NONE', 'WORKASPACE' ) );
#20497 = CIRCLE ( 'NONE', #13076, 11.23082370883260772 ) ;
#20498 = CARTESIAN_POINT ( 'NONE',  ( 3.000000000000000888, 111.0000000000000000, 80.99999999999998579 ) ) ;
#20499 = PRODUCT_DEFINITION_SHAPE ( 'NONE', 'NONE',  #16898 ) ;
#20500 = ORIENTED_EDGE ( 'NONE', *, *, #18054, .T. ) ;
#20501 = CARTESIAN_POINT ( 'NONE',  ( -7.022953521755574080, 5.102474405759713783, -9.433165578109189653 ) ) ;
#20502 = CONICAL_SURFACE ( 'NONE', #17376, 1.999999999999996669, 1.029744258676653867 ) ;
#20503 = CARTESIAN_POINT ( 'NONE',  ( 31.10231664966676846, 45.36128193761570770, 12.00000000000000000 ) ) ;
#20504 = AXIS2_PLACEMENT_3D ( 'NONE', #14922, #14702, #1543 ) ;
#20505 = ORIENTED_EDGE ( 'NONE', *, *, #10015, .T. ) ;
#20506 = EDGE_CURVE ( 'NONE', #16565, #10152, #1099, .T. ) ;
#20507 = DIRECTION ( 'NONE',  ( 0.000000000000000000, -6.938893903907222067E-15, 1.000000000000000000 ) ) ;
#20508 = VERTEX_POINT ( 'NONE', #8519 ) ;
#20509 = DIRECTION ( 'NONE',  ( 0.000000000000000000, -1.000000000000000000, 0.000000000000000000 ) ) ;
#20510 = VERTEX_POINT ( 'NONE', #15962 ) ;
#20511 = ADVANCED_FACE ( 'NONE', ( #6698 ), #13398, .T. ) ;
#20512 = CARTESIAN_POINT ( 'NONE',  ( 23.00000000000000000, 0.000000000000000000, 0.000000000000000000 ) ) ;
#20513 = DIRECTION ( 'NONE',  ( -0.000000000000000000, -0.000000000000000000, -1.000000000000000000 ) ) ;
#20514 = CARTESIAN_POINT ( 'NONE',  ( -29.00000000000000000, 29.49999999999999645, 0.000000000000000000 ) ) ;
#20515 = EDGE_CURVE ( 'NONE', #8450, #5111, #6002, .T. ) ;
#20516 = CARTESIAN_POINT ( 'NONE',  ( -34.00000000000000000, -3.851859888774471706E-31, 9.500000000000000000 ) ) ;
#20517 = ADVANCED_FACE ( 'NONE', ( #22190 ), #5627, .F. ) ;
#20518 = CIRCLE ( 'NONE', #18946, 1.999999999999996669 ) ;
#20519 = ADVANCED_FACE ( 'NONE', ( #22073 ), #18391, .T. ) ;
#20520 =( GEOMETRIC_REPRESENTATION_CONTEXT ( 3 ) GLOBAL_UNCERTAINTY_ASSIGNED_CONTEXT ( ( #22797 ) ) GLOBAL_UNIT_ASSIGNED_CONTEXT ( ( #17906, #23405, #3372 ) ) REPRESENTATION_CONTEXT ( 'NONE', 'WORKASPACE' ) );
#20521 = CIRCLE ( 'NONE', #23649, 5.000000000000007994 ) ;
#20522 = LINE ( 'NONE', #22474, #9820 ) ;
#20523 = CARTESIAN_POINT ( 'NONE',  ( 71.09090909090909349, 4.172000000000015696, 0.000000000000000000 ) ) ;
#20524 = CIRCLE ( 'NONE', #8426, 5.000000000000007994 ) ;
#20525 = CARTESIAN_POINT ( 'NONE',  ( -7.685661446562381371, 5.583959896777970222, -8.859589141758144493 ) ) ;
#20526 = ORIENTED_EDGE ( 'NONE', *, *, #11828, .T. ) ;
#20527 = FACE_OUTER_BOUND ( 'NONE', #10134, .T. ) ;
#20528 = CARTESIAN_POINT ( 'NONE',  ( 0.000000000000000000, 0.000000000000000000, 0.000000000000000000 ) ) ;
#20529 = VERTEX_POINT ( 'NONE', #9233 ) ;
#20530 = CARTESIAN_POINT ( 'NONE',  ( -5.871322893124554021, 8.081182679343978492, 5.906742014460232504 ) ) ;
#20531 = DIRECTION ( 'NONE',  ( -1.000000000000000000, -1.224606353822377258E-16, -0.000000000000000000 ) ) ;
#20532 = ORIENTED_EDGE ( 'NONE', *, *, #9021, .T. ) ;
#20533 = AXIS2_PLACEMENT_3D ( 'NONE', #15616, #21265, #4561 ) ;
#20534 = DIRECTION ( 'NONE',  ( -0.1313947906041722513, -0.9913301211009810654, 0.000000000000000000 ) ) ;
#20535 = CARTESIAN_POINT ( 'NONE',  ( 23.00000000000000000, -10.66755332433018744, -4.772587172891147311 ) ) ;
#20536 = CARTESIAN_POINT ( 'NONE',  ( -2.682529543899159208, -8.255977015246598327, -8.033165578109189298 ) ) ;
#20537 = EDGE_CURVE ( 'NONE', #14709, #4272, #1465, .T. ) ;
#20538 = DIRECTION ( 'NONE',  ( 0.000000000000000000, -1.000000000000000000, 0.000000000000000000 ) ) ;
#20539 = ORIENTED_EDGE ( 'NONE', *, *, #6715, .F. ) ;
#20540 = CARTESIAN_POINT ( 'NONE',  ( 8.871028110654306076, 6.042456644462176420E-13, 12.50000000000000000 ) ) ;
#20541 = FACE_OUTER_BOUND ( 'NONE', #14777, .T. ) ;
#20542 = CYLINDRICAL_SURFACE ( 'NONE', #15033, 6.050000000006050982 ) ;
#20543 = CARTESIAN_POINT ( 'NONE',  ( 39.00000000000000000, 29.49999999999999645, 12.00000000000000000 ) ) ;
#20544 = ORIENTED_EDGE ( 'NONE', *, *, #13976, .T. ) ;
#20545 = ADVANCED_FACE ( 'NONE', ( #11044 ), #20343, .T. ) ;
#20546 = ORIENTED_EDGE ( 'NONE', *, *, #8893, .F. ) ;
#20547 = EDGE_CURVE ( 'NONE', #779, #13326, #14604, .T. ) ;
#20548 = VERTEX_POINT ( 'NONE', #12772 ) ;
#20549 = ORIENTED_EDGE ( 'NONE', *, *, #11558, .F. ) ;
#20550 = ORIENTED_EDGE ( 'NONE', *, *, #21104, .F. ) ;
#20551 = DIRECTION ( 'NONE',  ( -0.000000000000000000, 0.000000000000000000, 1.000000000000000000 ) ) ;
#20552 = DIRECTION ( 'NONE',  ( 1.000000000000000000, 0.000000000000000000, 0.000000000000000000 ) ) ;
#20553 = CARTESIAN_POINT ( 'NONE',  ( 0.000000000000000000, -0.09016380984471504545, 11.68615217844040721 ) ) ;
#20554 = ORIENTED_EDGE ( 'NONE', *, *, #18228, .T. ) ;
#20555 = CARTESIAN_POINT ( 'NONE',  ( 1.999999999999994449, 45.00000000000000000, -26.97499999999999432 ) ) ;
#20556 = ORIENTED_EDGE ( 'NONE', *, *, #17813, .T. ) ;
#20557 = DIRECTION ( 'NONE',  ( -0.5735764363510517105, -0.8191520442889879128, 0.000000000000000000 ) ) ;
#20558 =( REPRESENTATION_RELATIONSHIP ('NONE','NONE', #21748, #9527 ) REPRESENTATION_RELATIONSHIP_WITH_TRANSFORMATION ( #5660 )SHAPE_REPRESENTATION_RELATIONSHIP( ) );
#20559 = DIRECTION ( 'NONE',  ( -0.000000000000000000, -0.000000000000000000, -1.000000000000000000 ) ) ;
#20560 = DIRECTION ( 'NONE',  ( 0.000000000000000000, 0.9096319953545194403, -0.4154150130018842146 ) ) ;
#20561 = CARTESIAN_POINT ( 'NONE',  ( 87.96568270381690979, 5.000000000000007105, 6.123233995736765296E-16 ) ) ;
#20562 = DIRECTION ( 'NONE',  ( 0.000000000000000000, 0.000000000000000000, 1.000000000000000000 ) ) ;
#20563 = ORIENTED_EDGE ( 'NONE', *, *, #9907, .T. ) ;
#20564 = DIRECTION ( 'NONE',  ( 0.000000000000000000, -1.000000000000000000, 0.000000000000000000 ) ) ;
#20565 = CARTESIAN_POINT ( 'NONE',  ( -30.16774287754690675, -40.66994976491903913, -3.000000000000000000 ) ) ;
#20566 = CARTESIAN_POINT ( 'NONE',  ( 0.000000000000000000, -15.03999999999999737, 0.000000000000000000 ) ) ;
#20567 = VERTEX_POINT ( 'NONE', #3396 ) ;
#20568 = CARTESIAN_POINT ( 'NONE',  ( -8.680847955711007202, -5.923547351154968927E-13, 5.633165578109188942 ) ) ;
#20569 = ORIENTED_EDGE ( 'NONE', *, *, #23762, .F. ) ;
#20570 = EDGE_CURVE ( 'NONE', #230, #17527, #21608, .T. ) ;
#20571 = APPLICATION_PROTOCOL_DEFINITION ( 'draft international standard', 'automotive_design', 1998, #18065 ) ;
#20572 = ORIENTED_EDGE ( 'NONE', *, *, #2684, .T. ) ;
#20573 = ORIENTED_EDGE ( 'NONE', *, *, #8619, .F. ) ;
#20574 = DIRECTION ( 'NONE',  ( 6.811450227741984732E-14, -1.000000000000000000, 0.000000000000000000 ) ) ;
#20575 = CARTESIAN_POINT ( 'NONE',  ( 2.682529543899157876, 8.255977015246598327, -9.033165578109187521 ) ) ;
#20576 = CARTESIAN_POINT ( 'NONE',  ( 84.76159002345582394, 7.562528597612068045E-15, 0.000000000000000000 ) ) ;
#20577 = ORIENTED_EDGE ( 'NONE', *, *, #18920, .F. ) ;
#20578 = DIRECTION ( 'NONE',  ( 4.613626265895764052E-16, 1.000000000000000000, -0.000000000000000000 ) ) ;
#20579 = CARTESIAN_POINT ( 'NONE',  ( -21.13207267780287069, -38.32709852940855910, 0.000000000000000000 ) ) ;
#20580 = AXIS2_PLACEMENT_3D ( 'NONE', #20223, #10909, #9098 ) ;
#20581 = CARTESIAN_POINT ( 'NONE',  ( 23.00000000000000000, -13.66196005206966468, 3.918670437617043145 ) ) ;
#20582 = CYLINDRICAL_SURFACE ( 'NONE', #2044, 5.000000000000000888 ) ;
#20583 = ORIENTED_EDGE ( 'NONE', *, *, #10546, .T. ) ;
#20584 = EDGE_CURVE ( 'NONE', #11167, #8265, #5100, .T. ) ;
#20585 = ORIENTED_EDGE ( 'NONE', *, *, #3479, .T. ) ;
#20586 = LINE ( 'NONE', #9583, #15255 ) ;
#20587 = CARTESIAN_POINT ( 'NONE',  ( -2.935661446562617183, 9.035036904803758873, -8.659589141758143427 ) ) ;
#20588 = PLANE ( 'NONE',  #10959 ) ;
#20589 = DIRECTION ( 'NONE',  ( 1.000000000000000000, 0.000000000000000000, 0.000000000000000000 ) ) ;
#20590 = DIRECTION ( 'NONE',  ( 0.000000000000000000, 0.000000000000000000, 1.000000000000000000 ) ) ;
#20591 = ADVANCED_FACE ( 'NONE', ( #5464 ), #1566, .T. ) ;
#20592 = CARTESIAN_POINT ( 'NONE',  ( -14.51962751333974389, 3.765689428759031010, 27.00000000000000000 ) ) ;
#20593 = LINE ( 'NONE', #15447, #7413 ) ;
#20594 = ORIENTED_EDGE ( 'NONE', *, *, #23362, .F. ) ;
#20595 = EDGE_CURVE ( 'NONE', #11678, #2779, #3273, .T. ) ;
#20596 = ORIENTED_EDGE ( 'NONE', *, *, #6372, .T. ) ;
#20597 = EDGE_CURVE ( 'NONE', #11492, #11172, #22004, .T. ) ;
#20598 = ORIENTED_EDGE ( 'NONE', *, *, #14454, .F. ) ;
#20599 = ORIENTED_EDGE ( 'NONE', *, *, #9085, .F. ) ;
#20600 =( GEOMETRIC_REPRESENTATION_CONTEXT ( 3 ) GLOBAL_UNCERTAINTY_ASSIGNED_CONTEXT ( ( #7644 ) ) GLOBAL_UNIT_ASSIGNED_CONTEXT ( ( #3554, #3451, #7561 ) ) REPRESENTATION_CONTEXT ( 'NONE', 'WORKASPACE' ) );
#20601 = VERTEX_POINT ( 'NONE', #22299 ) ;
#20602 = FACE_OUTER_BOUND ( 'NONE', #22271, .T. ) ;
#20603 = CARTESIAN_POINT ( 'NONE',  ( -31.74999999999995737, 0.000000000000000000, 0.000000000000000000 ) ) ;
#20604 = CARTESIAN_POINT ( 'NONE',  ( 27.70933665152130843, -40.41277845351217479, 12.00000000000000000 ) ) ;
#20605 = DIRECTION ( 'NONE',  ( -0.000000000000000000, -0.000000000000000000, -1.000000000000000000 ) ) ;
#20606 =( NAMED_UNIT ( * ) SI_UNIT ( $, .STERADIAN. ) SOLID_ANGLE_UNIT ( ) );
#20607 = LINE ( 'NONE', #2045, #21935 ) ;
#20608 = ORIENTED_EDGE ( 'NONE', *, *, #8287, .F. ) ;
#20609 = CARTESIAN_POINT ( 'NONE',  ( 1.255262969126036846E-16, -14.99147757894464306, 8.775000000000000355 ) ) ;
#20610 = EDGE_CURVE ( 'NONE', #8445, #19153, #9900, .T. ) ;
#20611 = DIRECTION ( 'NONE',  ( 0.000000000000000000, 0.000000000000000000, 1.000000000000000000 ) ) ;
#20612 = DIRECTION ( 'NONE',  ( -1.000000000000000000, -0.000000000000000000, -0.000000000000000000 ) ) ;
#20613 = CARTESIAN_POINT ( 'NONE',  ( -16.18147534945000032, 6.260849737139246862, -7.148624562014530781 ) ) ;
#20614 = LINE ( 'NONE', #3893, #17300 ) ;
#20615 = EDGE_CURVE ( 'NONE', #13428, #20777, #9513, .T. ) ;
#20616 = VERTEX_POINT ( 'NONE', #7040 ) ;
#20617 = ADVANCED_FACE ( 'NONE', ( #5225 ), #21232, .T. ) ;
#20618 = EDGE_LOOP ( 'NONE', ( #21787, #9780, #18670, #6352 ) ) ;
#20619 = DIRECTION ( 'NONE',  ( 0.000000000000000000, -0.000000000000000000, -1.000000000000000000 ) ) ;
#20620 = EDGE_LOOP ( 'NONE', ( #16872, #16736, #1049, #8478 ) ) ;
#20621 = DIRECTION ( 'NONE',  ( -0.000000000000000000, -0.000000000000000000, -1.000000000000000000 ) ) ;
#20622 = ORIENTED_EDGE ( 'NONE', *, *, #2579, .F. ) ;
#20623 = CARTESIAN_POINT ( 'NONE',  ( 34.10000000000000142, 29.50000000000000355, 0.000000000000000000 ) ) ;
#20624 = CARTESIAN_POINT ( 'NONE',  ( -40.00000000000000000, 0.000000000000000000, 12.00000000000000000 ) ) ;
#20625 = CARTESIAN_POINT ( 'NONE',  ( -23.85000000000000497, 15.03999999999999915, -25.00000000000000000 ) ) ;
#20626 = CARTESIAN_POINT ( 'NONE',  ( 33.25000000000000000, 29.50000000000000000, -2.224999999999995204 ) ) ;
#20627 = CARTESIAN_POINT ( 'NONE',  ( -2.935661446561384391, -9.035036904804158553, -7.459589141758144137 ) ) ;
#20628 = ORIENTED_EDGE ( 'NONE', *, *, #21457, .T. ) ;
#20629 = DIRECTION ( 'NONE',  ( 0.000000000000000000, 0.000000000000000000, 1.000000000000000000 ) ) ;
#20630 = CARTESIAN_POINT ( 'NONE',  ( -20.84999999999999787, 16.67999999999985405, 13.50000000000000178 ) ) ;
#20631 = EDGE_LOOP ( 'NONE', ( #19119, #873, #23187, #13230, #10689, #4697 ) ) ;
#20632 = FACE_BOUND ( 'NONE', #4200, .T. ) ;
#20633 = AXIS2_PLACEMENT_3D ( 'NONE', #18259, #12499, #19857 ) ;
#20634 = CARTESIAN_POINT ( 'NONE',  ( 0.000000000000000000, 0.000000000000000000, 0.000000000000000000 ) ) ;
#20635 = CARTESIAN_POINT ( 'NONE',  ( 15.00000000000000000, 5.618453542512190434E-15, -9.499999999999987566 ) ) ;
#20636 = VECTOR ( 'NONE', #19114, 1000.000000000000000 ) ;
#20637 = EDGE_CURVE ( 'NONE', #16656, #15558, #10573, .T. ) ;
#20638 = CARTESIAN_POINT ( 'NONE',  ( -2.901769741831041305, 8.519474286710609690, 80.21333227949575928 ) ) ;
#20639 = EDGE_CURVE ( 'NONE', #20648, #13451, #7288, .T. ) ;
#20640 = LINE ( 'NONE', #12941, #18038 ) ;
#20641 = CARTESIAN_POINT ( 'NONE',  ( 71.96568270381689558, 7.420530141404717394E-15, 0.000000000000000000 ) ) ;
#20642 = CARTESIAN_POINT ( 'NONE',  ( 17.25000000000000000, 15.50000000000000178, 14.70000000000000284 ) ) ;
#20643 = ORIENTED_EDGE ( 'NONE', *, *, #992, .T. ) ;
#20644 = DIRECTION ( 'NONE',  ( 0.000000000000000000, -0.5000000000000013323, -0.8660254037844379305 ) ) ;
#20645 = DIRECTION ( 'NONE',  ( 1.000000000000000000, 0.000000000000000000, -0.000000000000000000 ) ) ;
#20646 = FACE_OUTER_BOUND ( 'NONE', #13197, .T. ) ;
#20647 = CARTESIAN_POINT ( 'NONE',  ( 0.000000000000000000, 15.23000000000000220, 27.00000000000000000 ) ) ;
#20648 = VERTEX_POINT ( 'NONE', #7167 ) ;
#20649 = ORIENTED_EDGE ( 'NONE', *, *, #16243, .F. ) ;
#20650 = VECTOR ( 'NONE', #17950, 1000.000000000000000 ) ;
#20651 = CONTEXT_DEPENDENT_SHAPE_REPRESENTATION ( #6374, #14107 ) ;
#20652 = VERTEX_POINT ( 'NONE', #1337 ) ;
#20653 = CARTESIAN_POINT ( 'NONE',  ( 2.454813078130514813E-15, -16.67999999999999972, 14.50000000000000000 ) ) ;
#20654 = CARTESIAN_POINT ( 'NONE',  ( 80.39795365981946418, 7.562528597612068045E-15, 0.000000000000000000 ) ) ;
#20655 = EDGE_CURVE ( 'NONE', #4077, #6367, #14579, .T. ) ;
#20656 = DIRECTION ( 'NONE',  ( 0.000000000000000000, -1.000000000000000000, 0.000000000000000000 ) ) ;
#20657 = EDGE_LOOP ( 'NONE', ( #15228, #3326 ) ) ;
#20658 = ORIENTED_EDGE ( 'NONE', *, *, #17512, .F. ) ;
#20659 = CARTESIAN_POINT ( 'NONE',  ( 29.00000000000000000, -29.50000000000000355, 0.000000000000000000 ) ) ;
#20660 = LINE ( 'NONE', #5532, #15509 ) ;
#20661 = ORIENTED_EDGE ( 'NONE', *, *, #23672, .T. ) ;
#20662 = DIRECTION ( 'NONE',  ( 0.000000000000000000, -1.000000000000000000, 0.000000000000000000 ) ) ;
#20663 = ADVANCED_FACE ( 'NONE', ( #8391 ), #4995, .T. ) ;
#20664 = VERTEX_POINT ( 'NONE', #23416 ) ;
#20665 = EDGE_CURVE ( 'NONE', #2943, #19190, #14123, .T. ) ;
#20666 = CARTESIAN_POINT ( 'NONE',  ( -41.99999999999999289, 0.000000000000000000, 0.000000000000000000 ) ) ;
#20667 = FACE_BOUND ( 'NONE', #5810, .T. ) ;
#20668 = CARTESIAN_POINT ( 'NONE',  ( 21.85000000000000497, -16.67999999999999616, 12.00000000000000000 ) ) ;
#20669 = DIRECTION ( 'NONE',  ( 0.7071067811865574537, 8.659560562355054885E-17, -0.7071067811865376918 ) ) ;
#20670 =( GEOMETRIC_REPRESENTATION_CONTEXT ( 3 ) GLOBAL_UNCERTAINTY_ASSIGNED_CONTEXT ( ( #2538 ) ) GLOBAL_UNIT_ASSIGNED_CONTEXT ( ( #11166, #14474, #8833 ) ) REPRESENTATION_CONTEXT ( 'NONE', 'WORKASPACE' ) );
#20671 = ORIENTED_EDGE ( 'NONE', *, *, #14219, .F. ) ;
#20672 = DIRECTION ( 'NONE',  ( 1.000000000000000000, 0.000000000000000000, 0.000000000000000000 ) ) ;
#20673 = DIRECTION ( 'NONE',  ( -1.000000000000000000, -0.000000000000000000, -0.000000000000000000 ) ) ;
#20674 = ORIENTED_EDGE ( 'NONE', *, *, #3577, .F. ) ;
#20675 = ORIENTED_EDGE ( 'NONE', *, *, #22969, .F. ) ;
#20676 = CARTESIAN_POINT ( 'NONE',  ( 5.365059087798938364, 7.384370330707087149, 6.933165578109188765 ) ) ;
#20677 = ORIENTED_EDGE ( 'NONE', *, *, #14008, .T. ) ;
#20678 = PRODUCT_CONTEXT ( 'NONE', #4507, 'mechanical' ) ;
#20679 = ORIENTED_EDGE ( 'NONE', *, *, #2761, .T. ) ;
#20680 = ORIENTED_EDGE ( 'NONE', *, *, #20547, .T. ) ;
#20681 = CARTESIAN_POINT ( 'NONE',  ( 2.570122167802765922, 0.000000000000000000, 9.725923461386811297 ) ) ;
#20682 = CARTESIAN_POINT ( 'NONE',  ( -7.022953521755574080, 5.102474405759713783, -7.433165578109188765 ) ) ;
#20683 = ADVANCED_FACE ( 'NONE', ( #23536 ), #20836, .F. ) ;
#20684 = CONICAL_SURFACE ( 'NONE', #6679, 4.172000000000008590, 0.9599310885968742602 ) ;
#20685 = VERTEX_POINT ( 'NONE', #3142 ) ;
#20686 = CARTESIAN_POINT ( 'NONE',  ( 41.00000000000000000, 4.999999999999986677, 10.49999999999999822 ) ) ;
#20687 = CARTESIAN_POINT ( 'NONE',  ( 58.87477361290780919, 7.420530141404717394E-15, 0.000000000000000000 ) ) ;
#20688 = CARTESIAN_POINT ( 'NONE',  ( 37.00000000000000711, 29.50000000000000355, 11.50000000000000000 ) ) ;
#20689 = DIRECTION ( 'NONE',  ( -0.000000000000000000, -0.000000000000000000, 1.000000000000000000 ) ) ;
#20690 = CYLINDRICAL_SURFACE ( 'NONE', #11597, 6.050000000006052758 ) ;
#20691 = VERTEX_POINT ( 'NONE', #15955 ) ;
#20692 = DIRECTION ( 'NONE',  ( -1.000000000000000000, -0.000000000000000000, -0.000000000000000000 ) ) ;
#20693 = ORIENTED_EDGE ( 'NONE', *, *, #16637, .F. ) ;
#20694 = DIRECTION ( 'NONE',  ( 0.000000000000000000, -1.000000000000000000, 0.000000000000000000 ) ) ;
#20695 = ADVANCED_FACE ( 'NONE', ( #23303 ), #19638, .F. ) ;
#20696 = CARTESIAN_POINT ( 'NONE',  ( 23.85000000000000497, 15.03999999999999915, -25.00000000000000000 ) ) ;
#20697 = DIRECTION ( 'NONE',  ( -1.000000000000000000, 0.000000000000000000, 0.000000000000000000 ) ) ;
#20698 = EDGE_CURVE ( 'NONE', #2350, #3850, #6814, .T. ) ;
#20699 = CARTESIAN_POINT ( 'NONE',  ( 39.00000000000000000, -28.80990663662251805, 11.00000000000000000 ) ) ;
#20700 = DIRECTION ( 'NONE',  ( -0.000000000000000000, 0.000000000000000000, 1.000000000000000000 ) ) ;
#20701 = CARTESIAN_POINT ( 'NONE',  ( 89.12522638709219791, 7.562528597612068045E-15, 0.000000000000000000 ) ) ;
#20702 = EDGE_LOOP ( 'NONE', ( #8332, #2897, #23314, #8155 ) ) ;
#20703 = VERTEX_POINT ( 'NONE', #4878 ) ;
#20704 = VECTOR ( 'NONE', #10475, 1000.000000000000114 ) ;
#20705 = VERTEX_POINT ( 'NONE', #17801 ) ;
#20706 = VECTOR ( 'NONE', #6911, 1000.000000000000000 ) ;
#20707 = ORIENTED_EDGE ( 'NONE', *, *, #11661, .T. ) ;
#20708 =( LENGTH_UNIT ( ) NAMED_UNIT ( * ) SI_UNIT ( .MILLI., .METRE. ) );
#20709 = ORIENTED_EDGE ( 'NONE', *, *, #1667, .T. ) ;
#20710 = DIRECTION ( 'NONE',  ( 1.000000000000000000, 0.000000000000000000, 0.000000000000000000 ) ) ;
#20711 = CARTESIAN_POINT ( 'NONE',  ( -27.89784171216405895, -41.49349862090491570, -3.000000000000000000 ) ) ;
#20712 = ADVANCED_FACE ( 'NONE', ( #10341 ), #13765, .T. ) ;
#20713 = CARTESIAN_POINT ( 'NONE',  ( -7.685661446561619314, -5.583959896779019161, -10.40674201446023339 ) ) ;
#20714 = DIRECTION ( 'NONE',  ( -0.000000000000000000, -0.000000000000000000, -1.000000000000000000 ) ) ;
#20715 = DIRECTION ( 'NONE',  ( 0.000000000000000000, 0.000000000000000000, -1.000000000000000000 ) ) ;
#20716 = CARTESIAN_POINT ( 'NONE',  ( -6.822232771736904647E-13, 9.988891130263535700, -5.706742014460233214 ) ) ;
#20717 = EDGE_CURVE ( 'NONE', #12170, #12203, #2134, .T. ) ;
#20718 = DIRECTION ( 'NONE',  ( -1.000000000000000000, 0.000000000000000000, 0.000000000000000000 ) ) ;
#20719 = ORIENTED_EDGE ( 'NONE', *, *, #6715, .T. ) ;
#20720 = CIRCLE ( 'NONE', #3961, 1.999999999999996669 ) ;
#20721 = EDGE_CURVE ( 'NONE', #18707, #13078, #1374, .T. ) ;
#20722 = CARTESIAN_POINT ( 'NONE',  ( -10.00000000000000000, 0.000000000000000000, 0.000000000000000000 ) ) ;
#20723 = CARTESIAN_POINT ( 'NONE',  ( 6.699999999999996625, 0.000000000000000000, 13.72592346138681130 ) ) ;
#20724 = EDGE_CURVE ( 'NONE', #20777, #13428, #5245, .T. ) ;
#20725 = CARTESIAN_POINT ( 'NONE',  ( -31.74999999999995737, 0.000000000000000000, 0.000000000000000000 ) ) ;
#20726 = DIRECTION ( 'NONE',  ( 0.000000000000000000, 0.000000000000000000, 1.000000000000000000 ) ) ;
#20727 = B_SPLINE_CURVE_WITH_KNOTS ( 'NONE', 3,
 ( #13633, #15461, #718, #2777, #6687, #21578, #2906, #13894 ),
 .UNSPECIFIED., .F., .F.,
 ( 4, 2, 2, 4 ),
 ( 0.000000000000000000, 0.001825626494867649361, 0.002738439742301474258, 0.003651252989735298722 ),
 .UNSPECIFIED. ) ;
#20728 = CARTESIAN_POINT ( 'NONE',  ( 80.69295543108962931, -4.999999999999989342, 0.000000000000000000 ) ) ;
#20729 = ORIENTED_EDGE ( 'NONE', *, *, #15336, .T. ) ;
#20730 = CARTESIAN_POINT ( 'NONE',  ( 23.00000000000000000, 0.000000000000000000, 0.000000000000000000 ) ) ;
#20731 = ORIENTED_EDGE ( 'NONE', *, *, #19437, .T. ) ;
#20732 = DIRECTION ( 'NONE',  ( -0.7071067811865331398, 8.659560562355110352E-17, -0.7071067811865620056 ) ) ;
#20733 = VERTEX_POINT ( 'NONE', #11922 ) ;
#20734 = CARTESIAN_POINT ( 'NONE',  ( -6.822232771736903637E-13, 9.988891130263535700, 8.559589141758145558 ) ) ;
#20735 = VERTEX_POINT ( 'NONE', #14242 ) ;
#20736 = CARTESIAN_POINT ( 'NONE',  ( -31.74999999999995737, 0.000000000000000000, 5.000000000000000888 ) ) ;
#20737 = CIRCLE ( 'NONE', #15652, 4.172000000000008590 ) ;
#20738 = DIRECTION ( 'NONE',  ( 1.000000000000000000, 0.000000000000000000, 0.000000000000000000 ) ) ;
#20739 = CIRCLE ( 'NONE', #3200, 4.172000000000008590 ) ;
#20740 = CARTESIAN_POINT ( 'NONE',  ( 0.000000000000000000, -45.00000000000000000, -23.99999999999999645 ) ) ;
#20741 = EDGE_CURVE ( 'NONE', #18900, #13451, #18876, .T. ) ;
#20742 = AXIS2_PLACEMENT_3D ( 'NONE', #16100, #21364, #6714 ) ;
#20743 = AXIS2_PLACEMENT_3D ( 'NONE', #4081, #13835, #415 ) ;
#20744 = VECTOR ( 'NONE', #10871, 1000.000000000000000 ) ;
#20745 = CARTESIAN_POINT ( 'NONE',  ( -1.999999999999994449, 45.00000000000000000, 27.00000000000000000 ) ) ;
#20746 = EDGE_CURVE ( 'NONE', #9207, #18239, #1739, .T. ) ;
#20747 = DIRECTION ( 'NONE',  ( 1.000000000000000000, 0.000000000000000000, -0.000000000000000000 ) ) ;
#20748 = ORIENTED_EDGE ( 'NONE', *, *, #9297, .T. ) ;
#20749 = LINE ( 'NONE', #147, #2397 ) ;
#20750 = ORIENTED_EDGE ( 'NONE', *, *, #10720, .F. ) ;
#20751 = DIRECTION ( 'NONE',  ( 0.000000000000000000, -1.000000000000000000, 0.000000000000000000 ) ) ;
#20752 = CARTESIAN_POINT ( 'NONE',  ( -40.99749999999999517, 1.163414459189984894E-15, -9.499999999999994671 ) ) ;
#20753 = FACE_BOUND ( 'NONE', #49, .T. ) ;
#20754 = VECTOR ( 'NONE', #833, 1000.000000000000000 ) ;
#20755 = CARTESIAN_POINT ( 'NONE',  ( 72.54545454545454675, -4.172000000000000597, 0.000000000000000000 ) ) ;
#20756 = VECTOR ( 'NONE', #5626, 1000.000000000000000 ) ;
#20757 = CYLINDRICAL_SURFACE ( 'NONE', #19060, 5.000000000000000888 ) ;
#20758 = CIRCLE ( 'NONE', #14906, 4.057500000000000107 ) ;
#20759 = CYLINDRICAL_SURFACE ( 'NONE', #14142, 4.499999999999997335 ) ;
#20760 = CIRCLE ( 'NONE', #10229, 5.000000000000007994 ) ;
#20761 = DIRECTION ( 'NONE',  ( 0.000000000000000000, 0.000000000000000000, 1.000000000000000000 ) ) ;
#20762 = AXIS2_PLACEMENT_3D ( 'NONE', #17457, #13436, #4553 ) ;
#20763 = DIRECTION ( 'NONE',  ( 0.000000000000000000, 0.000000000000000000, 1.000000000000000000 ) ) ;
#20764 = ORIENTED_EDGE ( 'NONE', *, *, #19464, .F. ) ;
#20765 = VECTOR ( 'NONE', #278, 1000.000000000000000 ) ;
#20766 = CARTESIAN_POINT ( 'NONE',  ( 61.48886275072855057, 7.562528597612068045E-15, 0.000000000000000000 ) ) ;
#20767 = B_SPLINE_CURVE_WITH_KNOTS ( 'NONE', 3,
 ( #18024, #23656, #1201, #4873 ),
 .UNSPECIFIED., .F., .F.,
 ( 4, 4 ),
 ( 0.000000000000000000, 0.1802218513154718038 ),
 .UNSPECIFIED. ) ;
#20768 = CYLINDRICAL_SURFACE ( 'NONE', #14873, 11.00000000000001066 ) ;
#20769 = VECTOR ( 'NONE', #15425, 1000.000000000000000 ) ;
#20770 = DIRECTION ( 'NONE',  ( 0.000000000000000000, -0.9898214418809341275, 0.1423148382732755679 ) ) ;
#20771 = FACE_OUTER_BOUND ( 'NONE', #8078, .T. ) ;
#20772 = EDGE_LOOP ( 'NONE', ( #4411, #3945, #17868, #11513 ) ) ;
#20773 = ORIENTED_EDGE ( 'NONE', *, *, #6766, .T. ) ;
#20774 = ORIENTED_EDGE ( 'NONE', *, *, #3122, .F. ) ;
#20775 = VECTOR ( 'NONE', #4969, 1000.000000000000000 ) ;
#20776 = EDGE_CURVE ( 'NONE', #10733, #22129, #14196, .T. ) ;
#20777 = VERTEX_POINT ( 'NONE', #13898 ) ;
#20779 = CIRCLE ( 'NONE', #12199, 6.050000000006050982 ) ;
#20778 = CARTESIAN_POINT ( 'NONE',  ( 0.000000000000000000, 0.000000000000000000, 27.00000000000000000 ) ) ;
#20780 = EDGE_CURVE ( 'NONE', #9461, #1347, #11445, .T. ) ;
#20781 = CIRCLE ( 'NONE', #2863, 4.999999999999997335 ) ;
#20782 = AXIS2_PLACEMENT_3D ( 'NONE', #6066, #20470, #13245 ) ;
#20783 = FACE_OUTER_BOUND ( 'NONE', #12993, .T. ) ;
#20784 = EDGE_LOOP ( 'NONE', ( #19680, #3500, #4210, #7654 ) ) ;
#20785 = ORIENTED_EDGE ( 'NONE', *, *, #11055, .T. ) ;
#20786 = VECTOR ( 'NONE', #21523, 1000.000000000000000 ) ;
#20787 = CARTESIAN_POINT ( 'NONE',  ( -31.74999999999995737, 0.000000000000000000, 0.000000000000000000 ) ) ;
#20788 = AXIS2_PLACEMENT_3D ( 'NONE', #9625, #22833, #7784 ) ;
#20789 = ORIENTED_EDGE ( 'NONE', *, *, #17791, .F. ) ;
#20790 = ORIENTED_EDGE ( 'NONE', *, *, #20420, .T. ) ;
#20791 = CARTESIAN_POINT ( 'NONE',  ( -9.500000000000000000, -6.482511860946779655E-13, 10.20674201446023233 ) ) ;
#20792 = DIRECTION ( 'NONE',  ( -0.7052211081716895924, -0.7089874389501510388, -0.000000000000000000 ) ) ;
#20793 = DIRECTION ( 'NONE',  ( 1.000000000000000000, 0.000000000000000000, 0.000000000000000000 ) ) ;
#20794 = CARTESIAN_POINT ( 'NONE',  ( 83.60204634018053582, 7.420530141404717394E-15, 0.000000000000000000 ) ) ;
#20795 = ORIENTED_EDGE ( 'NONE', *, *, #7427, .T. ) ;
#20796 = CIRCLE ( 'NONE', #14550, 1.000000000000000888 ) ;
#20797 = CYLINDRICAL_SURFACE ( 'NONE', #12986, 4.499999999999997335 ) ;
#20798 = LINE ( 'NONE', #9668, #18826 ) ;
#20799 = ORIENTED_EDGE ( 'NONE', *, *, #15610, .T. ) ;
#20800 = CIRCLE ( 'NONE', #16509, 8.000000000000003553 ) ;
#20801 = EDGE_LOOP ( 'NONE', ( #23286, #13203, #11118, #15293 ) ) ;
#20802 = CARTESIAN_POINT ( 'NONE',  ( -8.680847955711200825, 2.820578480813073607, 5.533165578109187521 ) ) ;
#20803 = EDGE_CURVE ( 'NONE', #17488, #18602, #4074, .T. ) ;
#20804 = ORIENTED_EDGE ( 'NONE', *, *, #24009, .T. ) ;
#20805 = VECTOR ( 'NONE', #16026, 1000.000000000000000 ) ;
#20806 = CIRCLE ( 'NONE', #23152, 6.050000000006051870 ) ;
#20807 = EDGE_LOOP ( 'NONE', ( #5436, #15499, #11529, #8608 ) ) ;
#20808 = AXIS2_PLACEMENT_3D ( 'NONE', #17021, #11887, #15167 ) ;
#20809 = DIRECTION ( 'NONE',  ( 1.000000000000000000, 0.000000000000000000, 0.000000000000000000 ) ) ;
#20810 = EDGE_CURVE ( 'NONE', #9630, #18856, #16069, .T. ) ;
#20811 = VECTOR ( 'NONE', #17542, 1000.000000000000000 ) ;
#20812 = EDGE_LOOP ( 'NONE', ( #6246, #13936, #15450, #23619 ) ) ;
#20813 = ORIENTED_EDGE ( 'NONE', *, *, #7420, .F. ) ;
#20814 = EDGE_CURVE ( 'NONE', #1231, #13221, #10203, .T. ) ;
#20815 = DIRECTION ( 'NONE',  ( 1.000000000000000000, 1.224606353822377258E-16, 0.000000000000000000 ) ) ;
#20816 = CARTESIAN_POINT ( 'NONE',  ( 6.222797240145152671E-13, -9.127583699786111282, -12.13316557810918717 ) ) ;
#20817 = EDGE_CURVE ( 'NONE', #21353, #4092, #23579, .T. ) ;
#20818 = EDGE_CURVE ( 'NONE', #1952, #13312, #23999, .T. ) ;
#20819 = CYLINDRICAL_SURFACE ( 'NONE', #14554, 5.000000000000000888 ) ;
#20820 = ORIENTED_EDGE ( 'NONE', *, *, #22889, .T. ) ;
#20821 = FACE_OUTER_BOUND ( 'NONE', #1264, .T. ) ;
#20822 = FACE_OUTER_BOUND ( 'NONE', #20001, .T. ) ;
#20823 = DIRECTION ( 'NONE',  ( -0.000000000000000000, -0.000000000000000000, -1.000000000000000000 ) ) ;
#20824 = DIRECTION ( 'NONE',  ( 0.7052211081716905916, 0.7089874389501501506, 0.000000000000000000 ) ) ;
#20825 = DIRECTION ( 'NONE',  ( -1.000000000000000000, -1.224606353822377258E-16, -0.000000000000000000 ) ) ;
#20826 = CARTESIAN_POINT ( 'NONE',  ( 5.000000000000000000, 0.000000000000000000, 0.000000000000000000 ) ) ;
#20827 = AXIS2_PLACEMENT_3D ( 'NONE', #5484, #24036, #18664 ) ;
#20828 = AXIS2_PLACEMENT_3D ( 'NONE', #2819, #13440, #392 ) ;
#20829 = VERTEX_POINT ( 'NONE', #11524 ) ;
#20830 = VECTOR ( 'NONE', #3579, 1000.000000000000000 ) ;
#20831 = DIRECTION ( 'NONE',  ( -1.000000000000000000, 0.000000000000000000, 0.000000000000000000 ) ) ;
#20832 = DIRECTION ( 'NONE',  ( 0.000000000000000000, -1.000000000000000000, 0.000000000000000000 ) ) ;
#20833 = AXIS2_PLACEMENT_3D ( 'NONE', #11606, #1984, #2114 ) ;
#20834 = LINE ( 'NONE', #17032, #17268 ) ;
#20835 = CARTESIAN_POINT ( 'NONE',  ( 16.68617496892350260, 7.233372502334339593, -6.175747996014759877 ) ) ;
#20836 = CONICAL_SURFACE ( 'NONE', #23949, 0.9999999999999991118, 1.029744258676654090 ) ;
#20837 = FACE_OUTER_BOUND ( 'NONE', #11442, .T. ) ;
#20838 = DIRECTION ( 'NONE',  ( 1.000000000000000000, 0.000000000000000000, 0.000000000000000000 ) ) ;
#20839 = FACE_OUTER_BOUND ( 'NONE', #22513, .T. ) ;
#20840 = VERTEX_POINT ( 'NONE', #18509 ) ;
#20841 = EDGE_CURVE ( 'NONE', #16095, #22169, #16897, .T. ) ;
#20842 = EDGE_LOOP ( 'NONE', ( #22288, #22625, #13153, #4214 ) ) ;
#20843 = ORIENTED_EDGE ( 'NONE', *, *, #23890, .T. ) ;
#20844 =( NAMED_UNIT ( * ) PLANE_ANGLE_UNIT ( ) SI_UNIT ( $, .RADIAN. ) );
#20845 = EDGE_CURVE ( 'NONE', #2809, #11886, #10295, .T. ) ;
#20846 = AXIS2_PLACEMENT_3D ( 'NONE', #6598, #23327, #13661 ) ;
#20847 = AXIS2_PLACEMENT_3D ( 'NONE', #2955, #16239, #10494 ) ;
#20848 = EDGE_LOOP ( 'NONE', ( #18044, #8028 ) ) ;
#20849 = CARTESIAN_POINT ( 'NONE',  ( 2.935661446562616295, -9.035036904803758873, 9.659589141758143427 ) ) ;
#20850 = UNCERTAINTY_MEASURE_WITH_UNIT (LENGTH_MEASURE( 1.000000000000000082E-05 ), #19253, 'distance_accuracy_value', 'NONE');
#20851 = EDGE_CURVE ( 'NONE', #5942, #12689, #2522, .T. ) ;
#20852 = CIRCLE ( 'NONE', #23593, 0.2999999999999999334 ) ;
#20853 = AXIS2_PLACEMENT_3D ( 'NONE', #9677, #21384, #23225 ) ;
#20854 = DIRECTION ( 'NONE',  ( -5.501724186093585079E-16, -1.000000000000000000, 0.000000000000000000 ) ) ;
#20855 = DIRECTION ( 'NONE',  ( -1.000000000000000000, -1.224606353822377258E-16, -0.000000000000000000 ) ) ;
#20856 = FACE_OUTER_BOUND ( 'NONE', #675, .T. ) ;
#20857 = DIRECTION ( 'NONE',  ( -1.000000000000000000, 0.000000000000000000, 0.000000000000000000 ) ) ;
#20858 = CIRCLE ( 'NONE', #11081, 8.999999999999994671 ) ;
#20859 = VECTOR ( 'NONE', #4372, 1000.000000000000000 ) ;
#20860 = LINE ( 'NONE', #21078, #9402 ) ;
#20861 = DIRECTION ( 'NONE',  ( -0.000000000000000000, -0.000000000000000000, -1.000000000000000000 ) ) ;
#20862 = CYLINDRICAL_SURFACE ( 'NONE', #3985, 9.000000000000000000 ) ;
#20863 = CARTESIAN_POINT ( 'NONE',  ( -41.99999999999999289, 25.93535998569253920, 27.00000000000000000 ) ) ;
#20864 = CARTESIAN_POINT ( 'NONE',  ( -31.74999999999995737, 0.000000000000000000, 0.000000000000000000 ) ) ;
#20865 = EDGE_LOOP ( 'NONE', ( #13128, #16539, #11627, #17982, #2643 ) ) ;
#20866 = AXIS2_PLACEMENT_3D ( 'NONE', #10990, #11967, #19320 ) ;
#20867 = DIRECTION ( 'NONE',  ( -1.000000000000000000, 0.000000000000000000, 0.000000000000000000 ) ) ;
#20868 = ORIENTED_EDGE ( 'NONE', *, *, #20746, .T. ) ;
#20869 = CONICAL_SURFACE ( 'NONE', #13450, 1.999999999999994449, 1.029744258676653201 ) ;
#20870 = ORIENTED_EDGE ( 'NONE', *, *, #21027, .T. ) ;
#20871 = CARTESIAN_POINT ( 'NONE',  ( 2.935661446561383503, 9.035036904804158553, 8.459589141758144137 ) ) ;
#20872 = AXIS2_PLACEMENT_3D ( 'NONE', #19152, #2199, #16954 ) ;
#20873 = EDGE_LOOP ( 'NONE', ( #17411, #7971, #5454, #4526 ) ) ;
#20874 = CIRCLE ( 'NONE', #10339, 5.000000000000007994 ) ;
#20875 = DIRECTION ( 'NONE',  ( 0.7071067811865456854, 8.659560562354910671E-17, -0.7071067811865493491 ) ) ;
#20876 = DIRECTION ( 'NONE',  ( 0.7071067811865444641, 8.659560562354895880E-17, -0.7071067811865505703 ) ) ;
#20877 = CARTESIAN_POINT ( 'NONE',  ( 85.05659179472598908, 7.420530141404717394E-15, 0.000000000000000000 ) ) ;
#20878 = EDGE_CURVE ( 'NONE', #1315, #16254, #13827, .T. ) ;
#20879 = CARTESIAN_POINT ( 'NONE',  ( 5.000000000000000000, 0.000000000000000000, 4.057500000000000107 ) ) ;
#20880 = DIRECTION ( 'NONE',  ( -1.000000000000000000, -1.224606353822377258E-16, -0.000000000000000000 ) ) ;
#20881 = CIRCLE ( 'NONE', #19725, 5.000000000000007994 ) ;
#20882 = CARTESIAN_POINT ( 'NONE',  ( 7.685661446562381371, -5.583959896777971110, -3.859589141758143604 ) ) ;
#20883 = ORIENTED_EDGE ( 'NONE', *, *, #19724, .F. ) ;
#20884 = CIRCLE ( 'NONE', #4130, 6.050000000006052758 ) ;
#20885 = DIRECTION ( 'NONE',  ( -0.000000000000000000, -0.000000000000000000, -1.000000000000000000 ) ) ;
#20886 = VECTOR ( 'NONE', #12846, 1000.000000000000114 ) ;
#20887 = ORIENTED_EDGE ( 'NONE', *, *, #18737, .T. ) ;
#20888 = CARTESIAN_POINT ( 'NONE',  ( 23.00000000000000000, 0.000000000000000000, 0.000000000000000000 ) ) ;
#20889 = CYLINDRICAL_SURFACE ( 'NONE', #7504, 15.00000000000000000 ) ;
#20890 = AXIS2_PLACEMENT_3D ( 'NONE', #5905, #2250, #9417 ) ;
#20891 =( BOUNDED_CURVE ( )  B_SPLINE_CURVE ( 2, ( #15002, #15115, #274, #13173, #9631, #18682, #5862, #9376, #7556 ),
 .UNSPECIFIED., .F., .T. ) 
 B_SPLINE_CURVE_WITH_KNOTS ( ( 3, 2, 2, 2, 3 ),
 ( 0.1207052568533188430, 0.1400000000000000133, 0.1600000000000000033, 0.1799999999999999933, 0.2000000000000000111 ),
 .UNSPECIFIED. ) 
 CURVE ( )  GEOMETRIC_REPRESENTATION_ITEM ( )  RATIONAL_B_SPLINE_CURVE ( ( 0.9966699465879109709, 0.9527824026605606900, 1.000000000000000000, 0.9510565162951535312, 1.000000000000000000, 0.9510565162951535312, 1.000000000000000000, 0.9510565162951535312, 1.000000000000000000 ) ) 
 REPRESENTATION_ITEM ( '' )  );
#20892 = CARTESIAN_POINT ( 'NONE',  ( 42.62132034355964549, 25.48082444701819682, 9.418351429901832011E-16 ) ) ;
#20893 = CARTESIAN_POINT ( 'NONE',  ( -2.999999999999999112, 8.485281374238567764, 80.99999999999998579 ) ) ;
#20894 = EDGE_CURVE ( 'NONE', #15347, #5011, #16927, .T. ) ;
#20895 = DIRECTION ( 'NONE',  ( -1.000000000000000000, 0.000000000000000000, 0.000000000000000000 ) ) ;
#20896 = CARTESIAN_POINT ( 'NONE',  ( 1.000000000000000222, 1.224646799147353454E-16, 3.699999999999998845 ) ) ;
#20897 = CARTESIAN_POINT ( 'NONE',  ( -34.00000000000000000, 4.999999999999999112, 10.49999999999999822 ) ) ;
#20898 = ORIENTED_EDGE ( 'NONE', *, *, #9226, .F. ) ;
#20899 = DIRECTION ( 'NONE',  ( -0.000000000000000000, 1.000000000000000000, -0.000000000000000000 ) ) ;
#20900 = ADVANCED_FACE ( 'NONE', ( #12872 ), #8753, .F. ) ;
#20901 = CARTESIAN_POINT ( 'NONE',  ( 5.365059087799947335, -7.384370330706356178, 8.333165578109188232 ) ) ;
#20902 = AXIS2_PLACEMENT_3D ( 'NONE', #13232, #9438, #16667 ) ;
#20903 = CARTESIAN_POINT ( 'NONE',  ( 41.00000000000000000, 3.999999999999987121, 10.49999999999999822 ) ) ;
#20904 = PRODUCT_DEFINITION_FORMATION_WITH_SPECIFIED_SOURCE ( 'ANY', '', #23684, .NOT_KNOWN. ) ;
#20905 = VECTOR ( 'NONE', #4707, 1000.000000000000000 ) ;
#20906 = LINE ( 'NONE', #19183, #10971 ) ;
#20907 = VECTOR ( 'NONE', #5234, 1000.000000000000000 ) ;
#20908 = ORIENTED_EDGE ( 'NONE', *, *, #5300, .T. ) ;
#20909 = DIRECTION ( 'NONE',  ( 0.000000000000000000, -1.000000000000000000, 0.000000000000000000 ) ) ;
#20910 = CARTESIAN_POINT ( 'NONE',  ( -2.935661446561384391, -9.035036904804158553, -12.60674201446023446 ) ) ;
#20911 = ORIENTED_EDGE ( 'NONE', *, *, #20481, .F. ) ;
#20912 = ORIENTED_EDGE ( 'NONE', *, *, #18066, .T. ) ;
#20913 = CIRCLE ( 'NONE', #16617, 13.72592346138681130 ) ;
#20914 = CARTESIAN_POINT ( 'NONE',  ( -28.99999999999999645, -29.50000000000000000, -2.224999999999995204 ) ) ;
#20915 = ORIENTED_EDGE ( 'NONE', *, *, #15456, .T. ) ;
#20916 = AXIS2_PLACEMENT_3D ( 'NONE', #15251, #4195, #15512 ) ;
#20917 = EDGE_LOOP ( 'NONE', ( #12727, #9283 ) ) ;
#20918 = DIRECTION ( 'NONE',  ( -1.000000000000000000, -0.000000000000000000, -0.000000000000000000 ) ) ;
#20919 = CARTESIAN_POINT ( 'NONE',  ( 0.000000000000000000, 0.000000000000000000, 0.000000000000000000 ) ) ;
#20920 = AXIS2_PLACEMENT_3D ( 'NONE', #10222, #21095, #4396 ) ;
#20921 = DIRECTION ( 'NONE',  ( 0.000000000000000000, 0.000000000000000000, 1.000000000000000000 ) ) ;
#20922 = PRODUCT_DEFINITION_CONTEXT ( 'detailed design', #13864, 'design' ) ;
#20923 = LINE ( 'NONE', #4206, #16118 ) ;
#20924 = ORIENTED_EDGE ( 'NONE', *, *, #768, .F. ) ;
#20925 = CARTESIAN_POINT ( 'NONE',  ( 24.75000000000000711, 29.50000000000000000, 14.00000000000000178 ) ) ;
#20926 = ADVANCED_FACE ( 'NONE', ( #16771 ), #9127, .T. ) ;
#20927 = LINE ( 'NONE', #19454, #21185 ) ;
#20928 = ADVANCED_FACE ( 'NONE', ( #15865 ), #5808, .T. ) ;
#20929 = CYLINDRICAL_SURFACE ( 'NONE', #14643, 11.68650000001168721 ) ;
#20930 = ORIENTED_EDGE ( 'NONE', *, *, #19851, .F. ) ;
#20931 = CIRCLE ( 'NONE', #11550, 1.500000000000001332 ) ;
#20932 = VERTEX_POINT ( 'NONE', #15170 ) ;
#20933 = CARTESIAN_POINT ( 'NONE',  ( -5.365059087799947335, 7.384370330706355290, 7.333165578109188232 ) ) ;
#20934 = ORIENTED_EDGE ( 'NONE', *, *, #69, .T. ) ;
#20935 = CARTESIAN_POINT ( 'NONE',  ( -20.85000000000000497, -15.03999999999999737, 2.200000000000000178 ) ) ;
#20936 = AXIS2_PLACEMENT_3D ( 'NONE', #23813, #7088, #7874 ) ;
#20937 = ORIENTED_EDGE ( 'NONE', *, *, #19099, .T. ) ;
#20938 = ORIENTED_EDGE ( 'NONE', *, *, #4432, .T. ) ;
#20939 = DIRECTION ( 'NONE',  ( 0.000000000000000000, -0.000000000000000000, -1.000000000000000000 ) ) ;
#20940 = CARTESIAN_POINT ( 'NONE',  ( 6.222797240145152671E-13, -9.127583699786111282, -4.133165578109187166 ) ) ;
#20941 = FACE_OUTER_BOUND ( 'NONE', #1242, .T. ) ;
#20942 = VERTEX_POINT ( 'NONE', #20456 ) ;
#20943 = LINE ( 'NONE', #4105, #552 ) ;
#20944 = LINE ( 'NONE', #9933, #15428 ) ;
#20945 = DIRECTION ( 'NONE',  ( 1.000000000000000000, -0.000000000000000000, -0.000000000000000000 ) ) ;
#20946 = ORIENTED_EDGE ( 'NONE', *, *, #13030, .T. ) ;
#20947 = CARTESIAN_POINT ( 'NONE',  ( -28.99999999999999645, 29.50000000000000000, -3.000000000000000000 ) ) ;
#20948 = DIRECTION ( 'NONE',  ( 0.000000000000000000, 0.000000000000000000, 1.000000000000000000 ) ) ;
#20949 = ADVANCED_FACE ( 'NONE', ( #3744 ), #11152, .T. ) ;
#20950 = CARTESIAN_POINT ( 'NONE',  ( 6.809999908187194197E-13, -9.988891130263535700, -7.559589141758143782 ) ) ;
#20951 = CARTESIAN_POINT ( 'NONE',  ( 3.000000000000003109, 8.485281374238567764, 105.0000000000000000 ) ) ;
#20952 = DIRECTION ( 'NONE',  ( 0.000000000000000000, 0.000000000000000000, 1.000000000000000000 ) ) ;
#20953 = DIRECTION ( 'NONE',  ( 1.000000000000000000, 0.000000000000000000, -0.000000000000000000 ) ) ;
#20954 = ADVANCED_FACE ( 'NONE', ( #11638 ), #2512, .T. ) ;
#20955 = CARTESIAN_POINT ( 'NONE',  ( 40.23082370883260239, 29.49999999999999645, -1.500000000000000000 ) ) ;
#20956 = EDGE_CURVE ( 'NONE', #4606, #13326, #17726, .T. ) ;
#20957 = CARTESIAN_POINT ( 'NONE',  ( 6.809999908187194197E-13, -9.988891130263535700, 8.706742014460232326 ) ) ;
#20958 = ORIENTED_EDGE ( 'NONE', *, *, #15981, .T. ) ;
#20959 = CARTESIAN_POINT ( 'NONE',  ( -7.022953521754877748, -5.102474405760673015, 11.83316557810918823 ) ) ;
#20960 = ORIENTED_EDGE ( 'NONE', *, *, #4991, .T. ) ;
#20961 = DIRECTION ( 'NONE',  ( 1.000000000000000000, 0.000000000000000000, 0.000000000000000000 ) ) ;
#20962 = DIRECTION ( 'NONE',  ( -0.000000000000000000, -0.000000000000000000, -1.000000000000000000 ) ) ;
#20963 = ORIENTED_EDGE ( 'NONE', *, *, #11662, .T. ) ;
#20964 = CARTESIAN_POINT ( 'NONE',  ( -2.935661446562617183, 9.035036904803758873, -10.65958914175814343 ) ) ;
#20965 = AXIS2_PLACEMENT_3D ( 'NONE', #14715, #22533, #12762 ) ;
#20966 = FACE_OUTER_BOUND ( 'NONE', #484, .T. ) ;
#20967 = CARTESIAN_POINT ( 'NONE',  ( 5.000000000000000000, 2.342598717236913153, 4.057500000000004547 ) ) ;
#20968 = CARTESIAN_POINT ( 'NONE',  ( 20.84999999999999432, -15.04000000000000448, 27.00000000000000000 ) ) ;
#20969 = ORIENTED_EDGE ( 'NONE', *, *, #14447, .T. ) ;
#20970 = DIRECTION ( 'NONE',  ( 0.8757121056631641531, 0.4828336235133042775, 0.000000000000000000 ) ) ;
#20971 = EDGE_CURVE ( 'NONE', #4938, #14296, #694, .T. ) ;
#20972 = CARTESIAN_POINT ( 'NONE',  ( 27.19186005726088240, 42.23865125093339401, 0.000000000000000000 ) ) ;
#20973 = VERTEX_POINT ( 'NONE', #12003 ) ;
#20974 = DIRECTION ( 'NONE',  ( -1.000000000000000000, -0.000000000000000000, -0.000000000000000000 ) ) ;
#20975 = DIRECTION ( 'NONE',  ( 1.000000000000000000, 0.000000000000000000, 0.000000000000000000 ) ) ;
#20976 = CARTESIAN_POINT ( 'NONE',  ( -14.80736872429922890, 4.130115634539730074, 8.564444421911371563 ) ) ;
#20977 = DIRECTION ( 'NONE',  ( 0.000000000000000000, 0.000000000000000000, 1.000000000000000000 ) ) ;
#20978 = ADVANCED_FACE ( 'NONE', ( #21176 ), #13729, .F. ) ;
#20979 = EDGE_CURVE ( 'NONE', #13946, #978, #7061, .T. ) ;
#20980 = CIRCLE ( 'NONE', #10452, 6.050000000006051870 ) ;
#20981 = AXIS2_PLACEMENT_3D ( 'NONE', #13065, #15231, #7682 ) ;
#20982 = ORIENTED_EDGE ( 'NONE', *, *, #9758, .F. ) ;
#20983 = ORIENTED_EDGE ( 'NONE', *, *, #6282, .T. ) ;
#20984 = CARTESIAN_POINT ( 'NONE',  ( -9.499999999999790390, -3.086737114213257804, 11.15958914175814520 ) ) ;
#20985 = CARTESIAN_POINT ( 'NONE',  ( -5.871322893123450015, -8.081182679344781405, 12.50674201446023481 ) ) ;
#20986 = ORIENTED_EDGE ( 'NONE', *, *, #10823, .T. ) ;
#20987 = FACE_OUTER_BOUND ( 'NONE', #8927, .T. ) ;
#20988 = DIRECTION ( 'NONE',  ( 3.469446951953610639E-15, 1.000000000000000000, -0.000000000000000000 ) ) ;
#20989 = CARTESIAN_POINT ( 'NONE',  ( 0.000000000000000000, 0.000000000000000000, -1.500000000000000000 ) ) ;
#20990 = ORIENTED_EDGE ( 'NONE', *, *, #11168, .T. ) ;
#20991 = LINE ( 'NONE', #2320, #22059 ) ;
#20992 = DIRECTION ( 'NONE',  ( -0.000000000000000000, -0.000000000000000000, -1.000000000000000000 ) ) ;
#20993 = DIRECTION ( 'NONE',  ( -1.000000000000000000, -1.224606353822377258E-16, -0.000000000000000000 ) ) ;
#20994 = CARTESIAN_POINT ( 'NONE',  ( 58.87477361290780919, 6.123233995736675563E-16, -5.000000000000007994 ) ) ;
#20995 = ORIENTED_EDGE ( 'NONE', *, *, #17628, .F. ) ;
#20996 = LINE ( 'NONE', #15367, #16465 ) ;
#20997 = VERTEX_POINT ( 'NONE', #7528 ) ;
#20998 = CARTESIAN_POINT ( 'NONE',  ( -8.945956657690407710, -2.657973477511877736, 12.17557883498289506 ) ) ;
#20999 = CARTESIAN_POINT ( 'NONE',  ( 1.513123620469492447, 8.879344224389656759, 78.38024625474098173 ) ) ;
#21000 = DIRECTION ( 'NONE',  ( 0.000000000000000000, 1.000000000000000000, 0.000000000000000000 ) ) ;
#21001 = DIRECTION ( 'NONE',  ( -1.000000000000000000, 0.000000000000000000, 0.000000000000000000 ) ) ;
#21002 = CARTESIAN_POINT ( 'NONE',  ( 41.50000000000000000, -27.79189783386526358, 27.00000000000000000 ) ) ;
#21003 = AXIS2_PLACEMENT_3D ( 'NONE', #4182, #11323, #17336 ) ;
#21004 = ADVANCED_FACE ( 'NONE', ( #22452 ), #23208, .T. ) ;
#21005 = CARTESIAN_POINT ( 'NONE',  ( 41.00000000000000000, 0.000000000000000000, 12.00000000000000000 ) ) ;
#21006 = DIRECTION ( 'NONE',  ( 1.000000000000000000, 0.000000000000000000, 0.000000000000000000 ) ) ;
#21007 = EDGE_CURVE ( 'NONE', #3277, #8063, #8894, .T. ) ;
#21008 = CARTESIAN_POINT ( 'NONE',  ( 9.499999999999790390, 3.086737114213260025, -5.306742014460231971 ) ) ;
#21009 = ORIENTED_EDGE ( 'NONE', *, *, #2035, .T. ) ;
#21010 = DIRECTION ( 'NONE',  ( 1.000000000000000000, 0.000000000000000000, 0.000000000000000000 ) ) ;
#21011 = CARTESIAN_POINT ( 'NONE',  ( -7.022953521755574080, 5.102474405759713783, 9.433165578109189653 ) ) ;
#21012 = CARTESIAN_POINT ( 'NONE',  ( 35.99999999999999289, 50.99999999999999289, 0.5000000000000000000 ) ) ;
#21013 = LINE ( 'NONE', #4305, #5938 ) ;
#21014 = APPLICATION_CONTEXT ( 'automotive_design' ) ;
#21015 = EDGE_LOOP ( 'NONE', ( #13511, #19353, #2459, #17459 ) ) ;
#21016 = ITEM_DEFINED_TRANSFORMATION ( 'NONE', 'NONE', #21304,  #8005 ) ;
#21017 = ORIENTED_EDGE ( 'NONE', *, *, #591, .F. ) ;
#21018 = CARTESIAN_POINT ( 'NONE',  ( 9.324366623732823450E-16, 6.000000000000000000, 80.99999999999998579 ) ) ;
#21019 = AXIS2_PLACEMENT_3D ( 'NONE', #1925, #13999, #8502 ) ;
#21020 = EDGE_CURVE ( 'NONE', #11678, #8867, #16700, .T. ) ;
#21021 = CARTESIAN_POINT ( 'NONE',  ( -7.685661446562381371, 5.583959896777970222, -10.00674201446023481 ) ) ;
#21022 = ORIENTED_EDGE ( 'NONE', *, *, #2573, .F. ) ;
#21023 = AXIS2_PLACEMENT_3D ( 'NONE', #13617, #7993, #13870 ) ;
#21024 = EDGE_CURVE ( 'NONE', #8523, #23486, #1391, .T. ) ;
#21025 = CARTESIAN_POINT ( 'NONE',  ( 0.3000000000000020983, 1.803405503031483077E-15, -14.72592346043842326 ) ) ;
#21026 = EDGE_LOOP ( 'NONE', ( #7527, #6061, #1189 ) ) ;
#21027 = EDGE_CURVE ( 'NONE', #6244, #5168, #10833, .T. ) ;
#21028 = EDGE_CURVE ( 'NONE', #2131, #16878, #11460, .T. ) ;
#21029 = ORIENTED_EDGE ( 'NONE', *, *, #5039, .F. ) ;
#21030 = DIRECTION ( 'NONE',  ( -1.000000000000000000, 0.000000000000000000, 0.000000000000000000 ) ) ;
#21031 = PLANE ( 'NONE',  #10976 ) ;
#21032 = FACE_OUTER_BOUND ( 'NONE', #19416, .T. ) ;
#21033 = LINE ( 'NONE', #4320, #21164 ) ;
#21034 = ORIENTED_EDGE ( 'NONE', *, *, #9138, .T. ) ;
#21035 = DIRECTION ( 'NONE',  ( 0.000000000000000000, 0.000000000000000000, -1.000000000000000000 ) ) ;
#21036 = CARTESIAN_POINT ( 'NONE',  ( 83.30704456891035647, 5.000000000000015987, 0.000000000000000000 ) ) ;
#21037 = DIRECTION ( 'NONE',  ( -0.000000000000000000, -0.000000000000000000, -1.000000000000000000 ) ) ;
#21038 = ORIENTED_EDGE ( 'NONE', *, *, #9315, .F. ) ;
#21039 = AXIS2_PLACEMENT_3D ( 'NONE', #12395, #21800, #5082 ) ;
#21040 = ORIENTED_EDGE ( 'NONE', *, *, #17133, .T. ) ;
#21041 = CARTESIAN_POINT ( 'NONE',  ( 6.809999908187194197E-13, -9.988891130263535700, 5.559589141758142894 ) ) ;
#21042 = ORIENTED_EDGE ( 'NONE', *, *, #10786, .T. ) ;
#21043 = EDGE_LOOP ( 'NONE', ( #2469, #2050, #7710, #10156, #15176, #5891, #14058, #6825, #8194, #5353, #10508, #22954, #1195, #6690, #14670, #11378, #20679, #12708, #23716, #20585, #12768, #17410, #8961, #5265 ) ) ;
#21044 = ORIENTED_EDGE ( 'NONE', *, *, #21387, .T. ) ;
#21045 = FACE_OUTER_BOUND ( 'NONE', #14285, .T. ) ;
#21046 = CARTESIAN_POINT ( 'NONE',  ( 8.680847955711007202, 5.912916378492122225E-13, -6.633165578109188942 ) ) ;
#21047 = CARTESIAN_POINT ( 'NONE',  ( 5.000000000000000000, -2.342598717236916261, -4.057499999999997442 ) ) ;
#21048 = VERTEX_POINT ( 'NONE', #14496 ) ;
#21049 = CARTESIAN_POINT ( 'NONE',  ( -28.99999999999999645, 29.50000000000000000, 14.00000000000000178 ) ) ;
#21050 = DIRECTION ( 'NONE',  ( -0.000000000000000000, -0.000000000000000000, -1.000000000000000000 ) ) ;
#21051 = LINE ( 'NONE', #15667, #18372 ) ;
#21052 = EDGE_CURVE ( 'NONE', #19404, #18868, #20490, .T. ) ;
#21053 = ORIENTED_EDGE ( 'NONE', *, *, #18306, .T. ) ;
#21054 = DIRECTION ( 'NONE',  ( -0.000000000000000000, -0.000000000000000000, -1.000000000000000000 ) ) ;
#21055 = PLANE ( 'NONE',  #20390 ) ;
#21056 = AXIS2_PLACEMENT_3D ( 'NONE', #35, #9522, #22242 ) ;
#21057 = VERTEX_POINT ( 'NONE', #5370 ) ;
#21058 = DIRECTION ( 'NONE',  ( -0.000000000000000000, -0.000000000000000000, 1.000000000000000000 ) ) ;
#21059 = CARTESIAN_POINT ( 'NONE',  ( 5.871322893123448239, 8.081182679344781405, -8.359589141758144493 ) ) ;
#21060 = FACE_OUTER_BOUND ( 'NONE', #24076, .T. ) ;
#21061 = CARTESIAN_POINT ( 'NONE',  ( -2.682529543899159208, -8.255977015246598327, -6.033165578109189298 ) ) ;
#21062 = CARTESIAN_POINT ( 'NONE',  ( 86.21613547800127719, 6.123233995736675563E-16, -5.000000000000007994 ) ) ;
#21063 = VERTEX_POINT ( 'NONE', #16578 ) ;
#21064 = ORIENTED_EDGE ( 'NONE', *, *, #8968, .F. ) ;
#21065 = CARTESIAN_POINT ( 'NONE',  ( -5.365059087798939252, -7.384370330707086261, 7.933165578109187877 ) ) ;
#21066 = VERTEX_POINT ( 'NONE', #24033 ) ;
#21067 = CARTESIAN_POINT ( 'NONE',  ( 693.7818939062882464, 888.4837211537977737, 1295.681724745928250 ) ) ;
#21068 = CARTESIAN_POINT ( 'NONE',  ( 87.09090909090909349, 4.172000000000015696, 0.000000000000000000 ) ) ;
#21069 = VERTEX_POINT ( 'NONE', #14748 ) ;
#21070 = DIRECTION ( 'NONE',  ( 0.000000000000000000, 0.000000000000000000, 1.000000000000000000 ) ) ;
#21071 = DIRECTION ( 'NONE',  ( -0.000000000000000000, -0.000000000000000000, -1.000000000000000000 ) ) ;
#21072 = CARTESIAN_POINT ( 'NONE',  ( -29.00000000000000000, 29.49999999999999645, 12.00000000000000000 ) ) ;
#21073 = ORIENTED_EDGE ( 'NONE', *, *, #8822, .F. ) ;
#21074 = EDGE_CURVE ( 'NONE', #18986, #15347, #7308, .T. ) ;
#21075 = EDGE_CURVE ( 'NONE', #5633, #2260, #13529, .T. ) ;
#21076 = ORIENTED_EDGE ( 'NONE', *, *, #17841, .F. ) ;
#21077 = DIRECTION ( 'NONE',  ( -1.000000000000000000, -0.000000000000000000, -0.000000000000000000 ) ) ;
#21078 = CARTESIAN_POINT ( 'NONE',  ( 42.00000000000000000, -5.000000000000015099, 11.00000000000000000 ) ) ;
#21079 = DIRECTION ( 'NONE',  ( 0.000000000000000000, 0.000000000000000000, 1.000000000000000000 ) ) ;
#21080 = LINE ( 'NONE', #3040, #23468 ) ;
#21081 = CARTESIAN_POINT ( 'NONE',  ( 0.000000000000000000, 0.000000000000000000, 15.50000000000000000 ) ) ;
#21082 = CYLINDRICAL_SURFACE ( 'NONE', #5592, 6.050000000006051870 ) ;
#21083 =( BOUNDED_CURVE ( )  B_SPLINE_CURVE ( 2, ( #7643, #7403, #4133, #9597, #20849, #3880, #11057, #2040, #16925, #9245, #16693 ),
 .UNSPECIFIED., .F., .T. ) 
 B_SPLINE_CURVE_WITH_KNOTS ( ( 3, 2, 2, 2, 2, 3 ),
 ( 0.2000000000000000111, 0.2200000000000000289, 0.2400000000000000466, 0.2600000000000000644, 0.2800000000000001377, 0.3000000000000000999 ),
 .UNSPECIFIED. ) 
 CURVE ( )  GEOMETRIC_REPRESENTATION_ITEM ( )  RATIONAL_B_SPLINE_CURVE ( ( 1.000000000000000000, 0.9510565162951535312, 1.000000000000000000, 0.9510565162951535312, 1.000000000000000000, 0.9510565162951535312, 1.000000000000000000, 0.9510565162951535312, 1.000000000000000000, 0.9510565162951533091, 1.000000000000000222 ) ) 
 REPRESENTATION_ITEM ( '' )  );
#21084 = AXIS2_PLACEMENT_3D ( 'NONE', #6438, #13744, #19376 ) ;
#21085 = CARTESIAN_POINT ( 'NONE',  ( -2.935661446561384391, -9.035036904804158553, 4.606742014460233570 ) ) ;
#21086 = EDGE_LOOP ( 'NONE', ( #9947, #6297, #10493 ) ) ;
#21087 = CIRCLE ( 'NONE', #3170, 4.999999999999997335 ) ;
#21088 = EDGE_LOOP ( 'NONE', ( #22629, #17437, #22380, #20622 ) ) ;
#21089 = ORIENTED_EDGE ( 'NONE', *, *, #3648, .F. ) ;
#21090 = CARTESIAN_POINT ( 'NONE',  ( 7.685661446561619314, 5.583959896779020049, 10.25958914175814485 ) ) ;
#21091 = CARTESIAN_POINT ( 'NONE',  ( -2.935661446562617183, 9.035036904803758873, 11.80674201446023375 ) ) ;
#21092 = VERTEX_POINT ( 'NONE', #15337 ) ;
#21093 = DIRECTION ( 'NONE',  ( 1.000000000000000000, 0.000000000000000000, 0.000000000000000000 ) ) ;
#21094 = ADVANCED_FACE ( 'NONE', ( #19027 ), #20086, .F. ) ;
#21095 = DIRECTION ( 'NONE',  ( 0.000000000000000000, 0.000000000000000000, 1.000000000000000000 ) ) ;
#21096 = CARTESIAN_POINT ( 'NONE',  ( 5.871322893123448239, 8.081182679344781405, 6.359589141758142716 ) ) ;
#21097 = EDGE_CURVE ( 'NONE', #23250, #17123, #5277, .T. ) ;
#21098 = AXIS2_PLACEMENT_3D ( 'NONE', #17303, #20974, #20611 ) ;
#21099 = CARTESIAN_POINT ( 'NONE',  ( 6.669109785867858520, -5.768629174198284915, -12.49999999999999645 ) ) ;
#21100 = FACE_OUTER_BOUND ( 'NONE', #419, .T. ) ;
#21101 = CARTESIAN_POINT ( 'NONE',  ( 60.03431729618309021, 7.562528597612068045E-15, 0.000000000000000000 ) ) ;
#21102 = EDGE_CURVE ( 'NONE', #10216, #16364, #4582, .T. ) ;
#21103 = AXIS2_PLACEMENT_3D ( 'NONE', #21870, #12576, #1854 ) ;
#21104 = EDGE_CURVE ( 'NONE', #11994, #10631, #22020, .T. ) ;
#21105 = CIRCLE ( 'NONE', #21503, 9.000000000000000000 ) ;
#21106 = CARTESIAN_POINT ( 'NONE',  ( 9.499999999999790390, 3.086737114213260025, -4.159589141758141650 ) ) ;
#21107 = ORIENTED_EDGE ( 'NONE', *, *, #21599, .F. ) ;
#21108 = LINE ( 'NONE', #5758, #19178 ) ;
#21109 = ORIENTED_EDGE ( 'NONE', *, *, #17396, .T. ) ;
#21110 = CARTESIAN_POINT ( 'NONE',  ( 2.124376461992584897, -8.795015941986886077, 12.46040265135714975 ) ) ;
#21111 = DIRECTION ( 'NONE',  ( -1.000000000000000000, -0.000000000000000000, 0.000000000000000000 ) ) ;
#21112 = FACE_BOUND ( 'NONE', #12082, .T. ) ;
#21113 = DIRECTION ( 'NONE',  ( -5.501724186093582121E-16, 1.000000000000000000, 0.000000000000000000 ) ) ;
#21114 = DIRECTION ( 'NONE',  ( -1.000000000000000000, -0.000000000000000000, -0.000000000000000000 ) ) ;
#21115 = DIRECTION ( 'NONE',  ( -1.000000000000000000, 0.000000000000000000, 0.000000000000000000 ) ) ;
#21116 = CARTESIAN_POINT ( 'NONE',  ( 20.99999999999999645, 29.50000000000000355, 11.50000000000000000 ) ) ;
#21117 = ORIENTED_EDGE ( 'NONE', *, *, #17150, .T. ) ;
#21118 = CARTESIAN_POINT ( 'NONE',  ( 9.500000000000000000, 6.470877716354879437E-13, -5.206742014460234103 ) ) ;
#21119 = CIRCLE ( 'NONE', #12536, 9.000000000000000000 ) ;
#21120 = EDGE_LOOP ( 'NONE', ( #19998, #4144, #2003, #8814, #4542, #15945 ) ) ;
#21121 = AXIS2_PLACEMENT_3D ( 'NONE', #22807, #22556, #17168 ) ;
#21122 = CARTESIAN_POINT ( 'NONE',  ( 7.000000000000000888, 1.803405503031483077E-15, -14.72592346043842326 ) ) ;
#21123 = CARTESIAN_POINT ( 'NONE',  ( 5.365059087799947335, -7.384370330706356178, 6.333165578109188232 ) ) ;
#21124 = AXIS2_PLACEMENT_3D ( 'NONE', #4011, #7310, #18303 ) ;
#21125 = AXIS2_PLACEMENT_3D ( 'NONE', #15360, #13792, #6345 ) ;
#21126 = DIRECTION ( 'NONE',  ( -0.000000000000000000, -0.000000000000000000, -1.000000000000000000 ) ) ;
#21127 = EDGE_CURVE ( 'NONE', #13806, #21420, #15577, .T. ) ;
#21128 = ORIENTED_EDGE ( 'NONE', *, *, #8497, .T. ) ;
#21129 = ORIENTED_EDGE ( 'NONE', *, *, #10199, .T. ) ;
#21130 = CARTESIAN_POINT ( 'NONE',  ( 0.000000000000000000, 0.000000000000000000, 11.00000000000000000 ) ) ;
#21131 = EDGE_CURVE ( 'NONE', #8700, #6008, #11295, .T. ) ;
#21132 = DIRECTION ( 'NONE',  ( -1.000000000000000000, -0.000000000000000000, -0.000000000000000000 ) ) ;
#21133 = ORIENTED_EDGE ( 'NONE', *, *, #12996, .F. ) ;
#21134 = VERTEX_POINT ( 'NONE', #4261 ) ;
#21135 = CARTESIAN_POINT ( 'NONE',  ( -9.250591143756309975, -1.553302072574070714, -12.15226205728695064 ) ) ;
#21136 = CIRCLE ( 'NONE', #22317, 11.22592346138681130 ) ;
#21137 = CIRCLE ( 'NONE', #3597, 5.000000000000007994 ) ;
#21138 = AXIS2_PLACEMENT_3D ( 'NONE', #21248, #10376, #999 ) ;
#21139 = CARTESIAN_POINT ( 'NONE',  ( -2.024999999999999911, 45.00000000000000000, -27.00000000000000000 ) ) ;
#21140 = AXIS2_PLACEMENT_3D ( 'NONE', #12112, #11421, #16930 ) ;
#21141 = ORIENTED_EDGE ( 'NONE', *, *, #23128, .T. ) ;
#21142 = VECTOR ( 'NONE', #23951, 1000.000000000000000 ) ;
#21143 = AXIS2_PLACEMENT_3D ( 'NONE', #15588, #18914, #22942 ) ;
#21144 = VERTEX_POINT ( 'NONE', #5964 ) ;
#21145 = DIRECTION ( 'NONE',  ( 0.000000000000000000, -1.000000000000000000, 0.000000000000000000 ) ) ;
#21146 = AXIS2_PLACEMENT_3D ( 'NONE', #13858, #4594, #11995 ) ;
#21147 = FACE_BOUND ( 'NONE', #15256, .T. ) ;
#21148 = DIRECTION ( 'NONE',  ( -0.8247505806839219300, 0.5654966663575777819, 0.000000000000000000 ) ) ;
#21149 = DIRECTION ( 'NONE',  ( -0.000000000000000000, -1.000000000000000000, -0.000000000000000000 ) ) ;
#21150 = VERTEX_POINT ( 'NONE', #6087 ) ;
#21151 = CARTESIAN_POINT ( 'NONE',  ( 60.03431729618309021, 7.562528597612068045E-15, 0.000000000000000000 ) ) ;
#21152 = DIRECTION ( 'NONE',  ( -1.000000000000000000, -1.224606353822377258E-16, -0.000000000000000000 ) ) ;
#21153 = EDGE_LOOP ( 'NONE', ( #6247, #4269, #20188, #771 ) ) ;
#21154 = VERTEX_POINT ( 'NONE', #11426 ) ;
#21155 = CARTESIAN_POINT ( 'NONE',  ( -5.871322893123450015, -8.081182679344781405, 5.359589141758144493 ) ) ;
#21156 = ORIENTED_EDGE ( 'NONE', *, *, #16646, .F. ) ;
#21157 = CIRCLE ( 'NONE', #19629, 4.999999999999997335 ) ;
#21158 = ORIENTED_EDGE ( 'NONE', *, *, #19546, .F. ) ;
#21159 = ADVANCED_FACE ( 'NONE', ( #22558 ), #16947, .T. ) ;
#21160 = CIRCLE ( 'NONE', #3242, 5.000000000000007994 ) ;
#21161 = VERTEX_POINT ( 'NONE', #13264 ) ;
#21162 = AXIS2_PLACEMENT_3D ( 'NONE', #22503, #18474, #1762 ) ;
#21163 = VECTOR ( 'NONE', #3869, 1000.000000000000000 ) ;
#21164 = VECTOR ( 'NONE', #9913, 1000.000000000000000 ) ;
#21165 = ORIENTED_EDGE ( 'NONE', *, *, #13728, .T. ) ;
#21166 = ADVANCED_FACE ( 'NONE', ( #4377 ), #11666, .T. ) ;
#21167 = ORIENTED_EDGE ( 'NONE', *, *, #18640, .T. ) ;
#21168 = LINE ( 'NONE', #19354, #1291 ) ;
#21169 = CARTESIAN_POINT ( 'NONE',  ( -8.680847955710813579, -2.820578480814258437, -5.733165578109188587 ) ) ;
#21170 = ADVANCED_FACE ( 'NONE', ( #13147 ), #19135, .T. ) ;
#21171 = AXIS2_PLACEMENT_3D ( 'NONE', #22124, #5393, #20273 ) ;
#21172 = ORIENTED_EDGE ( 'NONE', *, *, #24032, .T. ) ;
#21173 = DIRECTION ( 'NONE',  ( 0.000000000000000000, 0.000000000000000000, -1.000000000000000000 ) ) ;
#21174 = LINE ( 'NONE', #2380, #11906 ) ;
#21175 = DIRECTION ( 'NONE',  ( 0.000000000000000000, 1.000000000000000000, 0.000000000000000000 ) ) ;
#21176 = FACE_OUTER_BOUND ( 'NONE', #2477, .T. ) ;
#21177 = CARTESIAN_POINT ( 'NONE',  ( -9.500000000000000000, -6.482511860946779655E-13, -9.059589141758143782 ) ) ;
#21178 = ORIENTED_EDGE ( 'NONE', *, *, #12004, .T. ) ;
#21179 = PLANE ( 'NONE',  #615 ) ;
#21180 = DIRECTION ( 'NONE',  ( 0.000000000000000000, 1.000000000000000000, 0.000000000000000000 ) ) ;
#21181 = ORIENTED_EDGE ( 'NONE', *, *, #9088, .F. ) ;
#21182 = DIRECTION ( 'NONE',  ( 0.8757121056631641531, -0.4828336235133042775, 0.000000000000000000 ) ) ;
#21183 = CYLINDRICAL_SURFACE ( 'NONE', #12504, 8.000000000000000000 ) ;
#21184 = AXIS2_PLACEMENT_3D ( 'NONE', #390, #18691, #7797 ) ;
#21185 = VECTOR ( 'NONE', #11620, 1000.000000000000000 ) ;
#21186 = CIRCLE ( 'NONE', #9859, 15.00000000000000000 ) ;
#21187 = CIRCLE ( 'NONE', #2071, 3.500000000000003109 ) ;
#21188 = DIRECTION ( 'NONE',  ( -1.000000000000000000, 0.000000000000000000, 0.000000000000000000 ) ) ;
#21189 = AXIS2_PLACEMENT_3D ( 'NONE', #7827, #2360, #16652 ) ;
#21190 = CARTESIAN_POINT ( 'NONE',  ( 2.682529543899157876, 8.255977015246598327, -5.033165578109189298 ) ) ;
#21191 = EDGE_CURVE ( 'NONE', #15047, #3047, #19267, .T. ) ;
#21192 = CIRCLE ( 'NONE', #21982, 8.000000000000003553 ) ;
#21193 = CARTESIAN_POINT ( 'NONE',  ( 61.48886275072855057, -5.000000000000000888, 6.123233995736776143E-16 ) ) ;
#21194 = ORIENTED_EDGE ( 'NONE', *, *, #18309, .F. ) ;
#21195 = ADVANCED_FACE ( 'NONE', ( #9838 ), #9966, .T. ) ;
#21196 = CARTESIAN_POINT ( 'NONE',  ( 5.365059087798938364, 7.384370330707087149, 8.933165578109186100 ) ) ;
#21197 = VERTEX_POINT ( 'NONE', #246 ) ;
#21198 = CARTESIAN_POINT ( 'NONE',  ( 693.7818939062881327, 888.4837211537981148, 1320.481724745928204 ) ) ;
#21199 = EDGE_CURVE ( 'NONE', #16945, #12085, #604, .T. ) ;
#21200 = CARTESIAN_POINT ( 'NONE',  ( 3.890962118697714531E-15, 15.50000000000000000, 7.699999999999998401 ) ) ;
#21201 = VERTEX_POINT ( 'NONE', #18765 ) ;
#21202 = CARTESIAN_POINT ( 'NONE',  ( -34.10000000000000142, 29.49999999999999645, 0.000000000000000000 ) ) ;
#21203 = CARTESIAN_POINT ( 'NONE',  ( -7.685661446561619314, -5.583959896779019161, -11.25958914175814307 ) ) ;
#21204 = AXIS2_PLACEMENT_3D ( 'NONE', #7668, #18434, #14993 ) ;
#21205 = CARTESIAN_POINT ( 'NONE',  ( 6.669109785867946449, -5.768629174198188103, 12.50000000000000533 ) ) ;
#21206 = CARTESIAN_POINT ( 'NONE',  ( -6.153822176767817416E-13, 9.500000000000000000, 3.706742014460231882 ) ) ;
#21207 = CYLINDRICAL_SURFACE ( 'NONE', #23601, 9.000000000000000000 ) ;
#21208 = CIRCLE ( 'NONE', #16136, 8.000000000000003553 ) ;
#21209 = CIRCLE ( 'NONE', #3291, 8.000000000000003553 ) ;
#21210 = VERTEX_POINT ( 'NONE', #2180 ) ;
#21211 = FACE_OUTER_BOUND ( 'NONE', #7045, .T. ) ;
#21212 = CARTESIAN_POINT ( 'NONE',  ( 0.000000000000000000, 2.119223430970397004, -17.74893002550478016 ) ) ;
#21213 = AXIS2_PLACEMENT_3D ( 'NONE', #16680, #3626, #10918 ) ;
#21214 = CARTESIAN_POINT ( 'NONE',  ( -31.74999999999995737, 0.000000000000000000, 5.000000000000000888 ) ) ;
#21215 = ORIENTED_EDGE ( 'NONE', *, *, #22673, .F. ) ;
#21216 = CARTESIAN_POINT ( 'NONE',  ( 19.85000000000000142, 16.67999999999999972, 13.50000000000000178 ) ) ;
#21217 = DIRECTION ( 'NONE',  ( 0.000000000000000000, -1.000000000000000000, 0.000000000000000000 ) ) ;
#21218 = CARTESIAN_POINT ( 'NONE',  ( -15.56475192642548855, 5.220978644676156577, 7.947934502462945083 ) ) ;
#21219 = DIRECTION ( 'NONE',  ( 0.000000000000000000, 0.000000000000000000, -1.000000000000000000 ) ) ;
#21220 = ORIENTED_EDGE ( 'NONE', *, *, #19235, .T. ) ;
#21221 = CARTESIAN_POINT ( 'NONE',  ( -7.022953521755574080, 5.102474405759713783, -3.433165578109189209 ) ) ;
#21222 = AXIS2_PLACEMENT_3D ( 'NONE', #3301, #8787, #21711 ) ;
#21223 = ORIENTED_EDGE ( 'NONE', *, *, #9676, .T. ) ;
#21224 = AXIS2_PLACEMENT_3D ( 'NONE', #5383, #18313, #20619 ) ;
#21225 = VERTEX_POINT ( 'NONE', #9607 ) ;
#21226 = CARTESIAN_POINT ( 'NONE',  ( -5.871322893123450015, -8.081182679344781405, 11.35958914175814272 ) ) ;
#21227 = EDGE_CURVE ( 'NONE', #16538, #2790, #10712, .T. ) ;
#21228 = CARTESIAN_POINT ( 'NONE',  ( -40.29291594121673370, -26.62062637246459218, 12.00000000000000000 ) ) ;
#21229 = ADVANCED_FACE ( 'NONE', ( #2258 ), #13483, .F. ) ;
#21230 = EDGE_LOOP ( 'NONE', ( #23025, #4223, #22250, #15475 ) ) ;
#21231 = CARTESIAN_POINT ( 'NONE',  ( 6.222797240145152671E-13, -9.127583699786111282, -12.13316557810918717 ) ) ;
#21232 = CONICAL_SURFACE ( 'NONE', #18493, 5.000000000000007994, 0.9599310885968855844 ) ;
#21233 = DIRECTION ( 'NONE',  ( -0.8660254037844385966, -0.5000000000000003331, 0.000000000000000000 ) ) ;
#21234 = CARTESIAN_POINT ( 'NONE',  ( 76.90909090909090651, 7.491529369508391930E-15, 0.000000000000000000 ) ) ;
#21235 = AXIS2_PLACEMENT_3D ( 'NONE', #8740, #8239, #1196 ) ;
#21236 = CARTESIAN_POINT ( 'NONE',  ( 5.000000000000000000, 4.685197434473818312, -1.301042606982605321E-15 ) ) ;
#21237 = DIRECTION ( 'NONE',  ( -0.000000000000000000, -0.000000000000000000, -1.000000000000000000 ) ) ;
#21238 = DIRECTION ( 'NONE',  ( 0.000000000000000000, -1.000000000000000000, 0.000000000000000000 ) ) ;
#21239 =( BOUNDED_CURVE ( )  B_SPLINE_CURVE ( 3, ( #19058, #20892, #11004, #16967 ),
 .UNSPECIFIED., .F., .T. ) 
 B_SPLINE_CURVE_WITH_KNOTS ( ( 4, 4 ),
 ( 4.712388980384688786, 6.283185307179586232 ),
 .UNSPECIFIED. ) 
 CURVE ( )  GEOMETRIC_REPRESENTATION_ITEM ( )  RATIONAL_B_SPLINE_CURVE ( ( 1.000000000000000000, 0.8047378541243648264, 0.8047378541243648264, 1.000000000000000000 ) ) 
 REPRESENTATION_ITEM ( '' )  );
#21240 = CARTESIAN_POINT ( 'NONE',  ( -20.85000000000000853, 15.04000000000000092, 25.00000000000000000 ) ) ;
#21241 = ORIENTED_EDGE ( 'NONE', *, *, #13954, .T. ) ;
#21242 = AXIS2_PLACEMENT_3D ( 'NONE', #4453, #23249, #1041 ) ;
#21243 = VERTEX_POINT ( 'NONE', #15891 ) ;
#21244 = CARTESIAN_POINT ( 'NONE',  ( -9.500000000000000000, -6.482511860946779655E-13, 9.059589141758143782 ) ) ;
#21245 = CARTESIAN_POINT ( 'NONE',  ( -3.205182335425767803, -8.579959099472988626, 12.34900154096814795 ) ) ;
#21246 = CIRCLE ( 'NONE', #10648, 4.172000000000008590 ) ;
#21247 = PRODUCT_DEFINITION ( 'UNKNOWN', '', #6092, #13334 ) ;
#21248 = CARTESIAN_POINT ( 'NONE',  ( 29.00000000000000711, -29.50000000000000711, 27.00000000000000000 ) ) ;
#21249 = CARTESIAN_POINT ( 'NONE',  ( -40.00000000000000000, 28.80990663662251450, 11.00000000000000000 ) ) ;
#21250 = EDGE_CURVE ( 'NONE', #18466, #16505, #21630, .T. ) ;
#21251 = VECTOR ( 'NONE', #6283, 1000.000000000000000 ) ;
#21252 = DIRECTION ( 'NONE',  ( -1.000000000000000000, 0.000000000000000000, 0.000000000000000000 ) ) ;
#21253 = ORIENTED_EDGE ( 'NONE', *, *, #16998, .T. ) ;
#21254 = FACE_OUTER_BOUND ( 'NONE', #7294, .T. ) ;
#21255 = DIRECTION ( 'NONE',  ( 1.000000000000000000, -0.000000000000000000, -0.000000000000000000 ) ) ;
#21256 = EDGE_CURVE ( 'NONE', #10579, #15563, #17127, .T. ) ;
#21257 = AXIS2_PLACEMENT_3D ( 'NONE', #21848, #23921, #7069 ) ;
#21258 = ORIENTED_EDGE ( 'NONE', *, *, #14801, .T. ) ;
#21259 = CARTESIAN_POINT ( 'NONE',  ( -2.935661446561384391, -9.035036904804158553, -4.606742014460233570 ) ) ;
#21260 = VERTEX_POINT ( 'NONE', #8443 ) ;
#21261 = CARTESIAN_POINT ( 'NONE',  ( 0.000000000000000000, 0.000000000000000000, -3.499999999999999556 ) ) ;
#21262 = CARTESIAN_POINT ( 'NONE',  ( 2.682529543900284974, -8.255977015246234174, 6.233165578109188587 ) ) ;
#21263 = EDGE_CURVE ( 'NONE', #4471, #15821, #10261, .T. ) ;
#21264 = EDGE_CURVE ( 'NONE', #13793, #23301, #4674, .T. ) ;
#21265 = DIRECTION ( 'NONE',  ( -1.000000000000000000, -0.000000000000000000, -0.000000000000000000 ) ) ;
#21266 = CARTESIAN_POINT ( 'NONE',  ( 6.250000000000000000, -10.82531754730548279, 2.500000000000000000 ) ) ;
#21267 = CARTESIAN_POINT ( 'NONE',  ( 61.48886275072855057, 7.562528597612068045E-15, 0.000000000000000000 ) ) ;
#21268 = AXIS2_PLACEMENT_3D ( 'NONE', #15218, #22691, #13418 ) ;
#21269 = ORIENTED_EDGE ( 'NONE', *, *, #8873, .F. ) ;
#21270 = VERTEX_POINT ( 'NONE', #15160 ) ;
#21271 = CARTESIAN_POINT ( 'NONE',  ( 0.000000000000000000, 0.000000000000000000, 0.000000000000000000 ) ) ;
#21272 = CIRCLE ( 'NONE', #16589, 4.999999999999997335 ) ;
#21273 = CIRCLE ( 'NONE', #3346, 6.050000000006051870 ) ;
#21274 = CARTESIAN_POINT ( 'NONE',  ( -9.500000000000000000, -6.482511860946779655E-13, -10.20674201446023233 ) ) ;
#21275 = EDGE_LOOP ( 'NONE', ( #19742, #4306, #17375, #15722, #18647, #12767, #4790, #21128, #16934, #14173, #2593, #9188, #22893, #14046, #10563, #1924, #7264, #7104, #11956, #16533 ) ) ;
#21276 = CARTESIAN_POINT ( 'NONE',  ( -5.294811499230706708, -7.532409217682791258, -12.30101643041108872 ) ) ;
#21277 = DIRECTION ( 'NONE',  ( 0.000000000000000000, 0.000000000000000000, 1.000000000000000000 ) ) ;
#21278 = ORIENTED_EDGE ( 'NONE', *, *, #15555, .F. ) ;
#21279 = EDGE_CURVE ( 'NONE', #4646, #19878, #4510, .T. ) ;
#21280 = ORIENTED_EDGE ( 'NONE', *, *, #14840, .F. ) ;
#21281 = AXIS2_PLACEMENT_3D ( 'NONE', #16062, #18023, #14459 ) ;
#21282 = DIRECTION ( 'NONE',  ( 0.000000000000000000, 0.000000000000000000, 1.000000000000000000 ) ) ;
#21283 = DIRECTION ( 'NONE',  ( 0.000000000000000000, -1.000000000000000000, 0.000000000000000000 ) ) ;
#21284 = DIRECTION ( 'NONE',  ( -1.000000000000000000, 0.000000000000000000, 0.000000000000000000 ) ) ;
#21285 = CIRCLE ( 'NONE', #11909, 4.499999999999997335 ) ;
#21286 = CARTESIAN_POINT ( 'NONE',  ( -30.16774287754692807, 40.66994976491904623, -3.000000000000000000 ) ) ;
#21287 = ORIENTED_EDGE ( 'NONE', *, *, #16336, .F. ) ;
#21288 = DIRECTION ( 'NONE',  ( -0.000000000000000000, -0.000000000000000000, -1.000000000000000000 ) ) ;
#21289 = DIRECTION ( 'NONE',  ( -0.000000000000000000, -0.000000000000000000, -1.000000000000000000 ) ) ;
#21290 = EDGE_CURVE ( 'NONE', #19427, #20703, #4896, .T. ) ;
#21291 = LINE ( 'NONE', #21655, #14263 ) ;
#21292 = EDGE_LOOP ( 'NONE', ( #1869, #19342, #9090 ) ) ;
#21293 = ADVANCED_FACE ( 'NONE', ( #2369 ), #4097, .T. ) ;
#21294 = AXIS2_PLACEMENT_3D ( 'NONE', #1598, #12920, #23805 ) ;
#21295 = ORIENTED_EDGE ( 'NONE', *, *, #20097, .F. ) ;
#21296 = CARTESIAN_POINT ( 'NONE',  ( -7.685661446561619314, -5.583959896779019161, 7.259589141758143960 ) ) ;
#21297 = ORIENTED_EDGE ( 'NONE', *, *, #4345, .F. ) ;
#21298 = ORIENTED_EDGE ( 'NONE', *, *, #4965, .F. ) ;
#21299 = ORIENTED_EDGE ( 'NONE', *, *, #14144, .T. ) ;
#21300 = ORIENTED_EDGE ( 'NONE', *, *, #23128, .F. ) ;
#21301 = DIRECTION ( 'NONE',  ( 0.000000000000000000, -1.000000000000000000, 0.000000000000000000 ) ) ;
#21302 = CARTESIAN_POINT ( 'NONE',  ( -5.365059087799947335, 7.384370330706355290, -5.333165578109189120 ) ) ;
#21303 = AXIS2_PLACEMENT_3D ( 'NONE', #5771, #11595, #38 ) ;
#21304 = AXIS2_PLACEMENT_3D ( 'NONE', #16189, #8501, #4864 ) ;
#21305 = CARTESIAN_POINT ( 'NONE',  ( 23.00000000000000000, -8.772759796005177080, -7.720943453482119523 ) ) ;
#21306 = DIRECTION ( 'NONE',  ( 1.000000000000000000, 0.000000000000000000, 0.000000000000000000 ) ) ;
#21307 = CONICAL_SURFACE ( 'NONE', #10757, 1.999999999999994449, 1.029744258676653201 ) ;
#21308 = ORIENTED_EDGE ( 'NONE', *, *, #1731, .F. ) ;
#21309 = CARTESIAN_POINT ( 'NONE',  ( -17.52920230446416738, -9.315347328456301312, -1.925892650121553196 ) ) ;
#21310 = DIRECTION ( 'NONE',  ( 0.000000000000000000, -1.000000000000000000, 0.000000000000000000 ) ) ;
#21311 = FACE_OUTER_BOUND ( 'NONE', #17851, .T. ) ;
#21312 = ORIENTED_EDGE ( 'NONE', *, *, #24038, .T. ) ;
#21313 = FACE_OUTER_BOUND ( 'NONE', #19831, .T. ) ;
#21314 = CARTESIAN_POINT ( 'NONE',  ( 9.500000000000000000, 6.470877716354879437E-13, 8.059589141758143782 ) ) ;
#21315 = VERTEX_POINT ( 'NONE', #12341 ) ;
#21316 = CARTESIAN_POINT ( 'NONE',  ( 0.6317332097108555589, -9.783628567664221620, 3.581108421866209479 ) ) ;
#21317 = CARTESIAN_POINT ( 'NONE',  ( 7.685661446561619314, 5.583959896779020049, 4.259589141758143960 ) ) ;
#21318 = LINE ( 'NONE', #11645, #19586 ) ;
#21319 = DIRECTION ( 'NONE',  ( -0.000000000000000000, 1.000000000000000000, -0.000000000000000000 ) ) ;
#21320 = CARTESIAN_POINT ( 'NONE',  ( 0.9999999999999986677, 0.000000000000000000, 0.000000000000000000 ) ) ;
#21321 = CARTESIAN_POINT ( 'NONE',  ( 8.680847955710813579, 2.820578480814259326, -6.733165578109188587 ) ) ;
#21322 = AXIS2_PLACEMENT_3D ( 'NONE', #20036, #10501, #16351 ) ;
#21323 = EDGE_CURVE ( 'NONE', #14561, #13101, #16549, .T. ) ;
#21324 = DIRECTION ( 'NONE',  ( -1.000000000000000000, -1.224606353822377258E-16, -0.000000000000000000 ) ) ;
#21325 = DIRECTION ( 'NONE',  ( -0.5735764363510517105, -0.8191520442889879128, 0.000000000000000000 ) ) ;
#21326 = ORIENTED_EDGE ( 'NONE', *, *, #10998, .F. ) ;
#21327 = EDGE_LOOP ( 'NONE', ( #11673, #2424, #21945, #15487 ) ) ;
#21328 = PRODUCT ( 'MAT-029', 'MAT-029', '', ( #12276 ) ) ;
#21329 = VERTEX_POINT ( 'NONE', #3082 ) ;
#21330 =( NAMED_UNIT ( * ) PLANE_ANGLE_UNIT ( ) SI_UNIT ( $, .RADIAN. ) );
#21331 = LINE ( 'NONE', #22919, #16329 ) ;
#21332 = ORIENTED_EDGE ( 'NONE', *, *, #11631, .F. ) ;
#21333 = FACE_OUTER_BOUND ( 'NONE', #4327, .T. ) ;
#21334 = FACE_OUTER_BOUND ( 'NONE', #16450, .T. ) ;
#21335 = UNCERTAINTY_MEASURE_WITH_UNIT (LENGTH_MEASURE( 1.000000000000000082E-05 ), #15070, 'distance_accuracy_value', 'NONE');
#21336 = CARTESIAN_POINT ( 'NONE',  ( -0.2004283449780275561, 8.999929632622238884, 101.9997888977613911 ) ) ;
#21337 = DIRECTION ( 'NONE',  ( 0.000000000000000000, 0.000000000000000000, 1.000000000000000000 ) ) ;
#21338 = DIRECTION ( 'NONE',  ( 1.000000000000000000, 1.224606353822377258E-16, 0.000000000000000000 ) ) ;
#21339 = ADVANCED_FACE ( 'NONE', ( #7837 ), #10503, .F. ) ;
#21340 = CYLINDRICAL_SURFACE ( 'NONE', #196, 1.000000000000000000 ) ;
#21341 = CARTESIAN_POINT ( 'NONE',  ( 0.000000000000000000, 0.000000000000000000, -12.00000000000000000 ) ) ;
#21342 = EDGE_CURVE ( 'NONE', #1993, #21134, #15282, .T. ) ;
#21343 = DIRECTION ( 'NONE',  ( -1.000000000000000000, 0.000000000000000000, 0.000000000000000000 ) ) ;
#21344 = CARTESIAN_POINT ( 'NONE',  ( 14.51962751333974389, -3.765689428759035895, 27.00000000000000000 ) ) ;
#21345 = CYLINDRICAL_SURFACE ( 'NONE', #18411, 9.000000000000001776 ) ;
#21346 = CARTESIAN_POINT ( 'NONE',  ( -28.27483331787887266, 41.23752903419610760, 27.00000000000000000 ) ) ;
#21347 =( REPRESENTATION_RELATIONSHIP ('NONE','NONE', #21748, #15960 ) REPRESENTATION_RELATIONSHIP_WITH_TRANSFORMATION ( #16633 )SHAPE_REPRESENTATION_RELATIONSHIP( ) );
#21348 = EDGE_CURVE ( 'NONE', #7111, #15532, #22759, .T. ) ;
#21349 = CYLINDRICAL_SURFACE ( 'NONE', #4468, 11.23082370883259706 ) ;
#21350 = ORIENTED_EDGE ( 'NONE', *, *, #7444, .F. ) ;
#21351 = CARTESIAN_POINT ( 'NONE',  ( -7.022953521755574080, 5.102474405759713783, -5.433165578109188765 ) ) ;
#21352 = VERTEX_POINT ( 'NONE', #13944 ) ;
#21353 = VERTEX_POINT ( 'NONE', #20935 ) ;
#21354 = CARTESIAN_POINT ( 'NONE',  ( -2.935661446561384391, -9.035036904804158553, 7.459589141758144137 ) ) ;
#21355 = CARTESIAN_POINT ( 'NONE',  ( -5.871322893124554021, 8.081182679343978492, 11.90674201446023339 ) ) ;
#21356 = AXIS2_PLACEMENT_3D ( 'NONE', #8921, #22001, #5283 ) ;
#21357 = VERTEX_POINT ( 'NONE', #17717 ) ;
#21358 =( LENGTH_UNIT ( ) NAMED_UNIT ( * ) SI_UNIT ( .MILLI., .METRE. ) );
#21359 = DIRECTION ( 'NONE',  ( -0.000000000000000000, -0.000000000000000000, -1.000000000000000000 ) ) ;
#21360 = CARTESIAN_POINT ( 'NONE',  ( -2.935661446562617183, 9.035036904803758873, 2.659589141758143871 ) ) ;
#21361 = DIRECTION ( 'NONE',  ( 0.000000000000000000, -0.000000000000000000, 1.000000000000000000 ) ) ;
#21362 = CARTESIAN_POINT ( 'NONE',  ( 14.91624121966758487, -1.615102390220943818, -9.367332145225617523 ) ) ;
#21363 = DIRECTION ( 'NONE',  ( -0.000000000000000000, -0.000000000000000000, -1.000000000000000000 ) ) ;
#21364 = DIRECTION ( 'NONE',  ( -0.000000000000000000, -0.000000000000000000, -1.000000000000000000 ) ) ;
#21365 = EDGE_CURVE ( 'NONE', #18928, #17223, #7957, .T. ) ;
#21366 = VERTEX_POINT ( 'NONE', #12213 ) ;
#21367 = EDGE_CURVE ( 'NONE', #19378, #977, #593, .T. ) ;
#21368 = EDGE_CURVE ( 'NONE', #1654, #8851, #1603, .T. ) ;
#21369 = ORIENTED_EDGE ( 'NONE', *, *, #16101, .F. ) ;
#21370 = DIRECTION ( 'NONE',  ( 1.000000000000000000, 0.000000000000000000, 0.000000000000000000 ) ) ;
#21371 = CARTESIAN_POINT ( 'NONE',  ( 0.000000000000000000, 1.374779123446053458E-15, -11.22592346138681130 ) ) ;
#21372 = CARTESIAN_POINT ( 'NONE',  ( 9.330908268522556170, -1.784418920662232289, 11.99999999999997691 ) ) ;
#21373 = CIRCLE ( 'NONE', #18249, 1.500000000000001332 ) ;
#21374 = LINE ( 'NONE', #17837, #21832 ) ;
#21375 = ORIENTED_EDGE ( 'NONE', *, *, #23948, .F. ) ;
#21376 = DIRECTION ( 'NONE',  ( -0.000000000000000000, -0.000000000000000000, 1.000000000000000000 ) ) ;
#21377 = ORIENTED_EDGE ( 'NONE', *, *, #17824, .F. ) ;
#21378 = CARTESIAN_POINT ( 'NONE',  ( -9.499999999999790390, -3.086737114213257804, -6.306742014460231971 ) ) ;
#21379 = EDGE_LOOP ( 'NONE', ( #5456, #9167, #23215 ) ) ;
#21380 = DIRECTION ( 'NONE',  ( -1.000000000000000000, 0.000000000000000000, 0.000000000000000000 ) ) ;
#21381 = CARTESIAN_POINT ( 'NONE',  ( 7.022953521754877748, 5.102474405760673903, 8.833165578109190008 ) ) ;
#21382 = CARTESIAN_POINT ( 'NONE',  ( 59.45454545454545325, 4.172000000000015696, 0.000000000000000000 ) ) ;
#21383 = DIRECTION ( 'NONE',  ( -0.000000000000000000, -0.000000000000000000, -1.000000000000000000 ) ) ;
#21384 = DIRECTION ( 'NONE',  ( -0.000000000000000000, -0.000000000000000000, -1.000000000000000000 ) ) ;
#21385 = CIRCLE ( 'NONE', #7714, 11.68650000001168721 ) ;
#21386 =( BOUNDED_SURFACE ( )  B_SPLINE_SURFACE ( 1, 2, ( 
 ( #22272, #11017, #22048, #12496, #18491, #3368, #21906, #23985, #19961, #5325, #8956, #16400, #8852, #7369, #20436, #16183, #6916, #18255, #12748, #3245, #5194, #3595, #16292, #12859, #23752, #1780, #5546, #12628, #23852, #10788, #24094, #10548, #9209, #10673, #18142, #1545, #1440, #16532, #22163, #7140, #18363, #5437, #20210, #3484, #10897, #1653, #9082, #7265, #14704, #20317, #71, #5795, #4212, #20933, #15156, #5685, #18981, #20676, #22520, #1997, #15417, #13222, #17246, #425, #548, #22887, #13108, #5908, #9559, #7474, #20568, #20802, #18847, #17009, #13341, #6158, #7723, #22403, #16754, #22628, #315, #4091, #3957, #11509, #2254, #18723, #14926, #11366, #2132, #7968, #9420, #3845, #9672, #17122, #11140, #11251, #3729 ),
 ( #16882, #2365, #7834, #15277, #22754, #198, #6036, #13478, #9779, #7604, #11623, #19091, #13596, #15049, #18616, #1897, #9311, #9921, #4591, #914, #6267, #793, #14079, #2625, #23376, #10034, #21528, #16022, #23117, #10153, #6403, #2992, #23482, #19713, #4831, #10417, #13846, #22997, #2858, #8469, #11989, #4699, #15915, #4328, #676, #12241, #12102, #17380, #21296, #21413, #15648, #8085, #19458, #17874, #1163, #8337, #13707, #19581, #2736, #17606, #19349, #8577, #15789, #6761, #17746, #21041, #11734, #21155, #23256, #6534, #15530, #4460, #13969, #10289, #1047, #6645, #19211, #2497, #11877, #17490, #8202, #23724, #6992, #3215, #20061, #14420, #6893, #19830, #18112, #1407, #9053, #21774, #17987, #21883, #16269, #21657, #10524 ) ),
 .UNSPECIFIED., .F., .F., .T. ) 
 B_SPLINE_SURFACE_WITH_KNOTS ( ( 2, 2 ),
 ( 3, 2, 2, 2, 2, 2, 2, 2, 2, 2, 2, 2, 2, 2, 2, 2, 2, 2, 2, 2, 2, 2, 2, 2, 2, 2, 2, 2, 2, 2, 2, 2, 2, 2, 2, 2, 2, 2, 2, 2, 2, 2, 2, 2, 2, 2, 2, 2, 3 ),
 ( 0.000000000000000000, 1.000000000000000000 ),
 ( 0.000000000000000000, 0.02000000000000000042, 0.04000000000000000083, 0.05999999999999999778, 0.08000000000000000167, 0.1000000000000000056, 0.1199999999999999956, 0.1400000000000000133, 0.1600000000000000033, 0.1799999999999999933, 0.2000000000000000111, 0.2200000000000000011, 0.2399999999999999911, 0.2600000000000000089, 0.2800000000000000266, 0.2999999999999999889, 0.3200000000000000067, 0.3400000000000000244, 0.3599999999999999867, 0.3800000000000000044, 0.4000000000000000222, 0.4199999999999999845, 0.4400000000000000022, 0.4600000000000000200, 0.4799999999999999822, 0.5000000000000000000, 0.5200000000000000178, 0.5400000000000000355, 0.5600000000000000533, 0.5799999999999999600, 0.5999999999999999778, 0.6199999999999999956, 0.6400000000000000133, 0.6600000000000000311, 0.6800000000000000488, 0.6999999999999999556, 0.7199999999999999734, 0.7399999999999999911, 0.7600000000000000089, 0.7800000000000000266, 0.8000000000000000444, 0.8199999999999999512, 0.8399999999999999689, 0.8599999999999999867, 0.8800000000000000044, 0.9000000000000000222, 0.9200000000000000400, 0.9399999999999999467, 0.9500000000000000666 ),
 .UNSPECIFIED. ) 
 GEOMETRIC_REPRESENTATION_ITEM ( )  RATIONAL_B_SPLINE_SURFACE ( (
 ( 1.000000000000000000, 0.9510565162951535312, 1.000000000000000000, 0.9510565162951535312, 1.000000000000000000, 0.9510565162951535312, 1.000000000000000000, 0.9510565162951535312, 1.000000000000000000, 0.9510565162951535312, 1.000000000000000000, 0.9510565162951535312, 1.000000000000000000, 0.9510565162951535312, 1.000000000000000000, 0.9510565162951535312, 1.000000000000000000, 0.9510565162951535312, 1.000000000000000000, 0.9510565162951535312, 1.000000000000000000, 0.9510565162951535312, 1.000000000000000000, 0.9510565162951535312, 1.000000000000000000, 0.9510565162951535312, 1.000000000000000000, 0.9510565162951535312, 1.000000000000000000, 0.9510565162951535312, 1.000000000000000000, 0.9510565162951535312, 1.000000000000000000, 0.9510565162951535312, 1.000000000000000000, 0.9510565162951535312, 1.000000000000000000, 0.9510565162951535312, 1.000000000000000000, 0.9510565162951535312, 1.000000000000000000, 0.9510565162951535312, 1.000000000000000000, 0.9510565162951535312, 1.000000000000000000, 0.9510565162951535312, 1.000000000000000000, 0.9510565162951535312, 1.000000000000000000, 0.9510565162951535312, 1.000000000000000000, 0.9510565162951535312, 1.000000000000000000, 0.9510565162951535312, 1.000000000000000000, 0.9510565162951535312, 1.000000000000000000, 0.9510565162951535312, 1.000000000000000000, 0.9510565162951535312, 1.000000000000000000, 0.9510565162951535312, 1.000000000000000000, 0.9510565162951535312, 1.000000000000000000, 0.9510565162951535312, 1.000000000000000000, 0.9510565162951535312, 1.000000000000000000, 0.9510565162951535312, 1.000000000000000000, 0.9510565162951535312, 1.000000000000000000, 0.9510565162951535312, 1.000000000000000000, 0.9510565162951535312, 1.000000000000000000, 0.9510565162951535312, 1.000000000000000000, 0.9510565162951535312, 1.000000000000000000, 0.9510565162951535312, 1.000000000000000000, 0.9510565162951535312, 1.000000000000000000, 0.9510565162951535312, 1.000000000000000000, 0.9510565162951535312, 1.000000000000000000, 0.9510565162951535312, 1.000000000000000000, 0.9510565162951535312, 1.000000000000000000, 0.9510565162951535312, 1.000000000000000000, 0.9755282581475764880, 0.9755282581475768211),
 ( 1.000000000000000000, 0.9510565162951535312, 1.000000000000000000, 0.9510565162951535312, 1.000000000000000000, 0.9510565162951535312, 1.000000000000000000, 0.9510565162951535312, 1.000000000000000000, 0.9510565162951535312, 1.000000000000000000, 0.9510565162951535312, 1.000000000000000000, 0.9510565162951535312, 1.000000000000000000, 0.9510565162951535312, 1.000000000000000000, 0.9510565162951535312, 1.000000000000000000, 0.9510565162951535312, 1.000000000000000000, 0.9510565162951535312, 1.000000000000000000, 0.9510565162951535312, 1.000000000000000000, 0.9510565162951535312, 1.000000000000000000, 0.9510565162951535312, 1.000000000000000000, 0.9510565162951535312, 1.000000000000000000, 0.9510565162951535312, 1.000000000000000000, 0.9510565162951535312, 1.000000000000000000, 0.9510565162951535312, 1.000000000000000000, 0.9510565162951535312, 1.000000000000000000, 0.9510565162951535312, 1.000000000000000000, 0.9510565162951535312, 1.000000000000000000, 0.9510565162951535312, 1.000000000000000000, 0.9510565162951535312, 1.000000000000000000, 0.9510565162951535312, 1.000000000000000000, 0.9510565162951535312, 1.000000000000000000, 0.9510565162951535312, 1.000000000000000000, 0.9510565162951535312, 1.000000000000000000, 0.9510565162951535312, 1.000000000000000000, 0.9510565162951535312, 1.000000000000000000, 0.9510565162951535312, 1.000000000000000000, 0.9510565162951535312, 1.000000000000000000, 0.9510565162951535312, 1.000000000000000000, 0.9510565162951535312, 1.000000000000000000, 0.9510565162951535312, 1.000000000000000000, 0.9510565162951535312, 1.000000000000000000, 0.9510565162951535312, 1.000000000000000000, 0.9510565162951535312, 1.000000000000000000, 0.9510565162951535312, 1.000000000000000000, 0.9510565162951535312, 1.000000000000000000, 0.9510565162951535312, 1.000000000000000000, 0.9510565162951535312, 1.000000000000000000, 0.9510565162951535312, 1.000000000000000000, 0.9510565162951535312, 1.000000000000000000, 0.9510565162951535312, 1.000000000000000000, 0.9510565162951535312, 1.000000000000000000, 0.9510565162951535312, 1.000000000000000000, 0.9510565162951535312, 1.000000000000000000, 0.9755282581475764880, 0.9755282581475768211) ) ) 
 REPRESENTATION_ITEM ( '' )  SURFACE ( )  );
#21387 = EDGE_CURVE ( 'NONE', #13548, #20120, #20461, .T. ) ;
#21388 = ORIENTED_EDGE ( 'NONE', *, *, #23391, .T. ) ;
#21389 = ITEM_DEFINED_TRANSFORMATION ( 'NONE', 'NONE', #628,  #8005 ) ;
#21390 = ORIENTED_EDGE ( 'NONE', *, *, #4552, .F. ) ;
#21391 = CARTESIAN_POINT ( 'NONE',  ( 0.000000000000000000, 0.000000000000000000, 0.000000000000000000 ) ) ;
#21392 = CARTESIAN_POINT ( 'NONE',  ( -31.74999999999995737, 0.000000000000000000, 5.000000000000000888 ) ) ;
#21393 = VERTEX_POINT ( 'NONE', #3439 ) ;
#21394 = DIRECTION ( 'NONE',  ( 0.000000000000000000, -1.000000000000000000, 0.000000000000000000 ) ) ;
#21395 = EDGE_CURVE ( 'NONE', #19319, #23989, #23979, .T. ) ;
#21396 = AXIS2_PLACEMENT_3D ( 'NONE', #21002, #2216, #8049 ) ;
#21397 = EDGE_CURVE ( 'NONE', #1596, #21725, #18438, .T. ) ;
#21398 = DIRECTION ( 'NONE',  ( -0.000000000000000000, 0.000000000000000000, 1.000000000000000000 ) ) ;
#21399 = VERTEX_POINT ( 'NONE', #22228 ) ;
#21400 = DIRECTION ( 'NONE',  ( 0.000000000000000000, 0.000000000000000000, -1.000000000000000000 ) ) ;
#21401 = EDGE_LOOP ( 'NONE', ( #15455, #1945, #8043, #14844 ) ) ;
#21402 = DIRECTION ( 'NONE',  ( 0.000000000000000000, -1.000000000000000000, 0.000000000000000000 ) ) ;
#21403 = CARTESIAN_POINT ( 'NONE',  ( 67.30704456891035647, 6.123233995736675563E-16, -5.000000000000007994 ) ) ;
#21404 = FACE_OUTER_BOUND ( 'NONE', #17040, .T. ) ;
#21405 = LINE ( 'NONE', #16014, #13387 ) ;
#21406=STYLED_ITEM('',(#24148),#2277);
#21407 = DIRECTION ( 'NONE',  ( 0.000000000000000000, -1.000000000000000000, 0.000000000000000000 ) ) ;
#21408 = ORIENTED_EDGE ( 'NONE', *, *, #13182, .T. ) ;
#21409 = DIRECTION ( 'NONE',  ( 1.000000000000000000, 0.000000000000000000, -0.000000000000000000 ) ) ;
#21410 = CARTESIAN_POINT ( 'NONE',  ( 0.000000000000000000, -14.80154252341802490, 10.02147513732818851 ) ) ;
#21411 = CARTESIAN_POINT ( 'NONE',  ( 2.935661446561383503, 9.035036904804158553, -4.459589141758144137 ) ) ;
#21412 = ORIENTED_EDGE ( 'NONE', *, *, #19413, .T. ) ;
#21413 = CARTESIAN_POINT ( 'NONE',  ( -9.499999999999790390, -3.086737114213257804, 7.159589141758144315 ) ) ;
#21414 = ORIENTED_EDGE ( 'NONE', *, *, #5965, .T. ) ;
#21415 = EDGE_CURVE ( 'NONE', #1690, #21063, #15388, .T. ) ;
#21416 = VERTEX_POINT ( 'NONE', #7324 ) ;
#21417 = CARTESIAN_POINT ( 'NONE',  ( -5.365059087798939252, -7.384370330707086261, -3.933165578109188321 ) ) ;
#21418 = CARTESIAN_POINT ( 'NONE',  ( 28.99999999999998934, -1.387778780781445676E-14, 10.49999999999999822 ) ) ;
#21419 = PLANE ( 'NONE',  #23100 ) ;
#21420 = VERTEX_POINT ( 'NONE', #21987 ) ;
#21421 = CARTESIAN_POINT ( 'NONE',  ( -17.57831567727900435, -9.462949834988608089, -0.9681625741885125924 ) ) ;
#21422 = AXIS2_PLACEMENT_3D ( 'NONE', #6659, #10305, #21426 ) ;
#21423 = ADVANCED_FACE ( 'NONE', ( #16127 ), #5296, .F. ) ;
#21424 = CARTESIAN_POINT ( 'NONE',  ( -19.84999999999999787, 16.67999999999999972, 13.50000000000000178 ) ) ;
#21425 = EDGE_CURVE ( 'NONE', #11173, #23706, #4914, .T. ) ;
#21426 = DIRECTION ( 'NONE',  ( 0.000000000000000000, 0.000000000000000000, -1.000000000000000000 ) ) ;
#21427 = ORIENTED_EDGE ( 'NONE', *, *, #13542, .F. ) ;
#21428 = CARTESIAN_POINT ( 'NONE',  ( 9.500000000000209610, -3.086737114211962396, -9.106742014460232681 ) ) ;
#21429 = DIRECTION ( 'NONE',  ( -1.000000000000000000, 0.000000000000000000, 0.000000000000000000 ) ) ;
#21430 = CARTESIAN_POINT ( 'NONE',  ( -6.153822176767817416E-13, 9.500000000000000000, 3.706742014460232326 ) ) ;
#21431 = CARTESIAN_POINT ( 'NONE',  ( 1.016919733032271456, 45.00000000000000000, 0.02500000000000418554 ) ) ;
#21432 = CARTESIAN_POINT ( 'NONE',  ( -41.73082370883260239, 27.62204025492845361, -1.500000000000000000 ) ) ;
#21433 = AXIS2_PLACEMENT_3D ( 'NONE', #23160, #6445, #19623 ) ;
#21434 = CARTESIAN_POINT ( 'NONE',  ( 23.85000000000000142, 15.03999999999999737, 0.000000000000000000 ) ) ;
#21435 = VECTOR ( 'NONE', #5073, 1000.000000000000000 ) ;
#21436 = DIRECTION ( 'NONE',  ( 0.000000000000000000, 0.000000000000000000, 1.000000000000000000 ) ) ;
#21437 = CARTESIAN_POINT ( 'NONE',  ( -7.022953521755574080, 5.102474405759713783, -9.433165578109189653 ) ) ;
#21438 = LINE ( 'NONE', #13878, #825 ) ;
#21439 = EDGE_LOOP ( 'NONE', ( #23054, #10474, #10759, #6511 ) ) ;
#21440 = ORIENTED_EDGE ( 'NONE', *, *, #3321, .F. ) ;
#21441 = CARTESIAN_POINT ( 'NONE',  ( 8.680847955711199049, -2.820578480813074496, 8.533165578109187521 ) ) ;
#21442 = VERTEX_POINT ( 'NONE', #24050 ) ;
#21443 = APPLICATION_PROTOCOL_DEFINITION ( 'draft international standard', 'automotive_design', 1998, #1971 ) ;
#21444 = EDGE_CURVE ( 'NONE', #4806, #14424, #5676, .T. ) ;
#21445 = CARTESIAN_POINT ( 'NONE',  ( 35.99999999999999289, 50.99999999999999289, 12.50000000000000000 ) ) ;
#21446 = EDGE_LOOP ( 'NONE', ( #20045, #19348, #11279, #366 ) ) ;
#21447 = ORIENTED_EDGE ( 'NONE', *, *, #16845, .T. ) ;
#21448 = CARTESIAN_POINT ( 'NONE',  ( 72.54545454545454675, 7.491529369508391930E-15, 0.000000000000000000 ) ) ;
#21449 = CARTESIAN_POINT ( 'NONE',  ( 7.685661446562381371, -5.583959896777971110, -11.85958914175814449 ) ) ;
#21450 = EDGE_CURVE ( 'NONE', #3540, #6174, #6465, .T. ) ;
#21451 = AXIS2_PLACEMENT_3D ( 'NONE', #5256, #23919, #18421 ) ;
#21452 = DIRECTION ( 'NONE',  ( -0.000000000000000000, -0.000000000000000000, -1.000000000000000000 ) ) ;
#21453 = CARTESIAN_POINT ( 'NONE',  ( 23.85000000000000497, 15.03999999999999915, 25.00000000000000000 ) ) ;
#21454 = DIRECTION ( 'NONE',  ( 0.8298699724181002324, 0.5579568342432785766, 1.919459897549205054E-15 ) ) ;
#21455 = EDGE_LOOP ( 'NONE', ( #17496, #7046, #3829, #5467, #5987 ) ) ;
#21456 = EDGE_CURVE ( 'NONE', #10212, #4272, #7595, .T. ) ;
#21457 = EDGE_CURVE ( 'NONE', #1690, #19902, #18320, .T. ) ;
#21458 = CYLINDRICAL_SURFACE ( 'NONE', #22703, 1.999999999999996669 ) ;
#21459 = CARTESIAN_POINT ( 'NONE',  ( 23.00000000000000000, 11.90821470209324140, 7.758837095328885880 ) ) ;
#21460 = CARTESIAN_POINT ( 'NONE',  ( 84.18181818181818699, -4.172000000000000597, 5.616230220889771312E-16 ) ) ;
#21461 = CARTESIAN_POINT ( 'NONE',  ( 5.000000000000000000, -2.342598717236905603, 4.057500000000010765 ) ) ;
#21462 = LINE ( 'NONE', #15959, #19565 ) ;
#21463 = CARTESIAN_POINT ( 'NONE',  ( 23.00000000000000000, 0.000000000000000000, 9.000000000000000000 ) ) ;
#21464 = ORIENTED_EDGE ( 'NONE', *, *, #17278, .T. ) ;
#21465 = CARTESIAN_POINT ( 'NONE',  ( -2.935661446561384391, -9.035036904804158553, -12.60674201446023446 ) ) ;
#21466 = EDGE_LOOP ( 'NONE', ( #19751, #7160, #10817, #6332 ) ) ;
#21467 = ORIENTED_EDGE ( 'NONE', *, *, #21263, .T. ) ;
#21468 = CIRCLE ( 'NONE', #16749, 5.000000000000007994 ) ;
#21469 = CARTESIAN_POINT ( 'NONE',  ( -2.935661446562617183, 9.035036904803758873, 2.659589141758143871 ) ) ;
#21470 = CARTESIAN_POINT ( 'NONE',  ( 0.000000000000000000, 0.000000000000000000, 15.50000000000000000 ) ) ;
#21471 = ADVANCED_FACE ( 'NONE', ( #6864 ), #16475, .T. ) ;
#21472 = ORIENTED_EDGE ( 'NONE', *, *, #10366, .F. ) ;
#21473 = FACE_OUTER_BOUND ( 'NONE', #20784, .T. ) ;
#21474 = EDGE_CURVE ( 'NONE', #13696, #18444, #1001, .T. ) ;
#21475 = CARTESIAN_POINT ( 'NONE',  ( -9.499999999999790390, -3.086737114213257804, 3.159589141758143871 ) ) ;
#21476 = PLANE ( 'NONE',  #8803 ) ;
#21477 = ORIENTED_EDGE ( 'NONE', *, *, #2367, .T. ) ;
#21478 = CARTESIAN_POINT ( 'NONE',  ( 77.48886275072855767, 5.000000000000015099, 0.000000000000000000 ) ) ;
#21479 = ADVANCED_FACE ( 'NONE', ( #5141 ), #14651, .F. ) ;
#21480 = LINE ( 'NONE', #15977, #5958 ) ;
#21481 = EDGE_CURVE ( 'NONE', #11467, #20276, #8912, .T. ) ;
#21482 = ORIENTED_EDGE ( 'NONE', *, *, #10149, .F. ) ;
#21483 = CIRCLE ( 'NONE', #20305, 4.172000000000008590 ) ;
#21484 = APPLICATION_CONTEXT ( 'automotive_design' ) ;
#21485 = ORIENTED_EDGE ( 'NONE', *, *, #1883, .F. ) ;
#21486 = CARTESIAN_POINT ( 'NONE',  ( 29.00000000000000355, 29.50000000000000000, -27.00000000000000000 ) ) ;
#21487 = CARTESIAN_POINT ( 'NONE',  ( 41.99999999999997158, -25.22443390181681622, -3.000000000000000000 ) ) ;
#21488 = DIRECTION ( 'NONE',  ( 1.000000000000000000, 0.000000000000000000, 0.000000000000000000 ) ) ;
#21489 = DIRECTION ( 'NONE',  ( -0.000000000000000000, -0.000000000000000000, -1.000000000000000000 ) ) ;
#21490 = ORIENTED_EDGE ( 'NONE', *, *, #13851, .F. ) ;
#21491 = CARTESIAN_POINT ( 'NONE',  ( -9.500000000000000000, -6.482511860946779655E-13, 9.059589141758143782 ) ) ;
#21492 = VERTEX_POINT ( 'NONE', #1250 ) ;
#21493 = DIRECTION ( 'NONE',  ( -0.000000000000000000, 0.000000000000000000, 1.000000000000000000 ) ) ;
#21494 = EDGE_LOOP ( 'NONE', ( #17739, #10408, #3681, #8185 ) ) ;
#21495 = CARTESIAN_POINT ( 'NONE',  ( -7.022953521754877748, -5.102474405760673015, 3.833165578109188676 ) ) ;
#21496 = ADVANCED_FACE ( 'NONE', ( #5392 ), #20869, .F. ) ;
#21497 = FACE_OUTER_BOUND ( 'NONE', #11100, .T. ) ;
#21498 = LINE ( 'NONE', #23457, #19588 ) ;
#21499 = CIRCLE ( 'NONE', #22259, 0.7000000000000005107 ) ;
#21500 = EDGE_CURVE ( 'NONE', #22436, #14296, #2170, .T. ) ;
#21501 = AXIS2_PLACEMENT_3D ( 'NONE', #20528, #20172, #14879 ) ;
#21502 = CARTESIAN_POINT ( 'NONE',  ( 6.809999908187194197E-13, -9.988891130263535700, 5.559589141758142894 ) ) ;
#21503 = AXIS2_PLACEMENT_3D ( 'NONE', #23394, #16042, #12127 ) ;
#21504 = ORIENTED_EDGE ( 'NONE', *, *, #16679, .T. ) ;
#21505 = CONTEXT_DEPENDENT_SHAPE_REPRESENTATION ( #22575, #7690 ) ;
#21506 = ORIENTED_EDGE ( 'NONE', *, *, #18556, .F. ) ;
#21507 = CARTESIAN_POINT ( 'NONE',  ( -30.16774287754692807, 40.66994976491904623, -3.000000000000000000 ) ) ;
#21508 = CARTESIAN_POINT ( 'NONE',  ( 7.685661446562381371, -5.583959896777971110, -7.006742014460233037 ) ) ;
#21509 = ORIENTED_EDGE ( 'NONE', *, *, #18143, .T. ) ;
#21510 = CARTESIAN_POINT ( 'NONE',  ( 3.239832068448452951, -8.450089895365024972, -12.48376408781543034 ) ) ;
#21511 = DIRECTION ( 'NONE',  ( -1.000000000000000000, 0.000000000000000000, 0.000000000000000000 ) ) ;
#21512 = VERTEX_POINT ( 'NONE', #3795 ) ;
#21513 = LINE ( 'NONE', #899, #11585 ) ;
#21514 = CIRCLE ( 'NONE', #6710, 11.68650000001168898 ) ;
#21515 = AXIS2_PLACEMENT_3D ( 'NONE', #15488, #9738, #22955 ) ;
#21516 = VERTEX_POINT ( 'NONE', #22349 ) ;
#21517 = DIRECTION ( 'NONE',  ( 0.000000000000000000, -1.000000000000000000, 0.000000000000000000 ) ) ;
#21518 = DIRECTION ( 'NONE',  ( -1.000000000000000000, -0.000000000000000000, -0.000000000000000000 ) ) ;
#21519 = PRODUCT_DEFINITION_SHAPE ( 'NONE', 'NONE',  #24114 ) ;
#21520 = CARTESIAN_POINT ( 'NONE',  ( 0.000000000000000000, 0.000000000000000000, 6.000000000000000000 ) ) ;
#21521 = CIRCLE ( 'NONE', #21914, 11.68650000001168721 ) ;
#21522 = DIRECTION ( 'NONE',  ( 0.000000000000000000, -1.000000000000000000, 0.000000000000000000 ) ) ;
#21523 = DIRECTION ( 'NONE',  ( 0.000000000000000000, -1.000000000000000000, 0.000000000000000000 ) ) ;
#21524 = ORIENTED_EDGE ( 'NONE', *, *, #12997, .F. ) ;
#21525 = LINE ( 'NONE', #11983, #173 ) ;
#21526 = CARTESIAN_POINT ( 'NONE',  ( 31.10231664966676846, -45.36128193761570770, -27.00000000000000000 ) ) ;
#21527 = FACE_OUTER_BOUND ( 'NONE', #15545, .T. ) ;
#21528 = CARTESIAN_POINT ( 'NONE',  ( -2.935661446561384391, -9.035036904804158553, 9.459589141758144137 ) ) ;
#21529 = B_SPLINE_CURVE_WITH_KNOTS ( 'NONE', 3,
 ( #21875, #14779, #22009, #12588, #5288, #9045, #12715, #20176 ),
 .UNSPECIFIED., .F., .F.,
 ( 4, 2, 2, 4 ),
 ( 0.000000000000000000, 0.001946159586596647381, 0.002919239379894971072, 0.003892319173193294762 ),
 .UNSPECIFIED. ) ;
#21530 = EDGE_CURVE ( 'NONE', #6705, #10396, #7548, .T. ) ;
#21531 = ORIENTED_EDGE ( 'NONE', *, *, #8845, .T. ) ;
#21532 = EDGE_CURVE ( 'NONE', #898, #12216, #3720, .T. ) ;
#21533 = CIRCLE ( 'NONE', #18781, 1.000000000000000888 ) ;
#21534 = ORIENTED_EDGE ( 'NONE', *, *, #3709, .T. ) ;
#21535 = VERTEX_POINT ( 'NONE', #13053 ) ;
#21536 = AXIS2_PLACEMENT_3D ( 'NONE', #5117, #14036, #10721 ) ;
#21537 = CIRCLE ( 'NONE', #10202, 6.050000000006050982 ) ;
#21539 = CIRCLE ( 'NONE', #8662, 18.50000000000000000 ) ;
#21538 = DIRECTION ( 'NONE',  ( 1.000000000000000000, 0.000000000000000000, 0.000000000000000000 ) ) ;
#21540 = VECTOR ( 'NONE', #13923, 1000.000000000000000 ) ;
#21541 = AXIS2_PLACEMENT_3D ( 'NONE', #907, #9770, #10023 ) ;
#21542 = DIRECTION ( 'NONE',  ( -0.000000000000000000, -0.000000000000000000, -1.000000000000000000 ) ) ;
#21543 = CARTESIAN_POINT ( 'NONE',  ( -1.029124893018731811E-15, -45.00000000000000000, 4.201721238055123209 ) ) ;
#21544 = CARTESIAN_POINT ( 'NONE',  ( -15.09475045435787699, -4.494086555308247632, 8.407297576120608795 ) ) ;
#21545 = CARTESIAN_POINT ( 'NONE',  ( 88.54545454545454675, 4.172000000000015696, 0.000000000000000000 ) ) ;
#21546 = ORIENTED_EDGE ( 'NONE', *, *, #15057, .F. ) ;
#21547 = DIRECTION ( 'NONE',  ( 1.000000000000000000, 0.000000000000000000, 0.000000000000000000 ) ) ;
#21548 = CARTESIAN_POINT ( 'NONE',  ( -6.250000000000000888, 10.82531754730548279, -2.500000000000000000 ) ) ;
#21549 = CARTESIAN_POINT ( 'NONE',  ( -7.685661446561619314, -5.583959896779019161, 4.406742014460233392 ) ) ;
#21550 = CARTESIAN_POINT ( 'NONE',  ( 9.500000000000209610, -3.086737114211962396, 3.959589141758144581 ) ) ;
#21551 = DIRECTION ( 'NONE',  ( 1.000000000000000000, 0.000000000000000000, 0.000000000000000000 ) ) ;
#21552 = DIRECTION ( 'NONE',  ( -0.000000000000000000, 1.000000000000000000, -0.000000000000000000 ) ) ;
#21553 = ADVANCED_FACE ( 'NONE', ( #14870 ), #5857, .T. ) ;
#21554 = DIRECTION ( 'NONE',  ( -0.000000000000000000, 1.000000000000000000, -0.000000000000000000 ) ) ;
#21555 = DIRECTION ( 'NONE',  ( -0.000000000000000000, -0.000000000000000000, -1.000000000000000000 ) ) ;
#21556 = CIRCLE ( 'NONE', #17249, 1.000000000000000888 ) ;
#21557 = AXIS2_PLACEMENT_3D ( 'NONE', #326, #7738, #22770 ) ;
#21558 = CIRCLE ( 'NONE', #12961, 40.00000000000000000 ) ;
#21559 = AXIS2_PLACEMENT_3D ( 'NONE', #20399, #3688, #1741 ) ;
#21560 = EDGE_CURVE ( 'NONE', #19949, #977, #20991, .T. ) ;
#21561 = ORIENTED_EDGE ( 'NONE', *, *, #15610, .F. ) ;
#21562 = CARTESIAN_POINT ( 'NONE',  ( -9.000000000000000000, 1.102182119232617714E-15, 0.9999999999999731326 ) ) ;
#21563 = VERTEX_POINT ( 'NONE', #4032 ) ;
#21564 = AXIS2_PLACEMENT_3D ( 'NONE', #15476, #17548, #6098 ) ;
#21565 = CARTESIAN_POINT ( 'NONE',  ( 5.365059087798938364, 7.384370330707087149, 6.933165578109188765 ) ) ;
#21566 = EDGE_CURVE ( 'NONE', #5235, #2368, #232, .T. ) ;
#21567 = EDGE_CURVE ( 'NONE', #12416, #3226, #14996, .T. ) ;
#21568 = EDGE_CURVE ( 'NONE', #9530, #15114, #18676, .T. ) ;
#21569 = AXIS2_PLACEMENT_3D ( 'NONE', #13486, #22527, #5801 ) ;
#21570 = ORIENTED_EDGE ( 'NONE', *, *, #19440, .T. ) ;
#21571 = APPLICATION_PROTOCOL_DEFINITION ( 'draft international standard', 'automotive_design', 1998, #4507 ) ;
#21572 = FACE_OUTER_BOUND ( 'NONE', #21829, .T. ) ;
#21573 = ORIENTED_EDGE ( 'NONE', *, *, #23483, .F. ) ;
#21574 = ORIENTED_EDGE ( 'NONE', *, *, #14351, .F. ) ;
#21575 = CARTESIAN_POINT ( 'NONE',  ( 0.000000000000000000, -45.00000000000000000, 0.000000000000000000 ) ) ;
#21576 = CARTESIAN_POINT ( 'NONE',  ( -9.500000000000000000, -6.482511860946779655E-13, -7.059589141758143782 ) ) ;
#21577 = CARTESIAN_POINT ( 'NONE',  ( 2.258892838145987181, 8.713070189660834686, 100.9838146350991934 ) ) ;
#21579 = VECTOR ( 'NONE', #4351, 1000.000000000000000 ) ;
#21578 = CARTESIAN_POINT ( 'NONE',  ( 8.199992213793651175, -2.961991314798469332, 12.49999999999999467 ) ) ;
#21580 = DIRECTION ( 'NONE',  ( 0.000000000000000000, 0.000000000000000000, 1.000000000000000000 ) ) ;
#21581 = TOROIDAL_SURFACE ( 'NONE', #9024, 10.00000000000000533, 1.000000000000000000 ) ;
#21582 = CIRCLE ( 'NONE', #152, 6.050000000006050982 ) ;
#21583 = AXIS2_PLACEMENT_3D ( 'NONE', #11275, #7507, #13378 ) ;
#21584 = FACE_OUTER_BOUND ( 'NONE', #7616, .T. ) ;
#21585 = CIRCLE ( 'NONE', #11019, 5.000000000000007994 ) ;
#21586 = DIRECTION ( 'NONE',  ( -1.000000000000000000, -1.224606353822377258E-16, -0.000000000000000000 ) ) ;
#21587 = LINE ( 'NONE', #8133, #9023 ) ;
#21588 = ORIENTED_EDGE ( 'NONE', *, *, #8736, .T. ) ;
#21589 = CARTESIAN_POINT ( 'NONE',  ( 77.48886275072855767, 7.562528597612068045E-15, 0.000000000000000000 ) ) ;
#21590 = AXIS2_PLACEMENT_3D ( 'NONE', #23910, #7185, #22093 ) ;
#21591 = DIRECTION ( 'NONE',  ( 0.000000000000000000, -0.4999999999999989453, 0.8660254037844392627 ) ) ;
#21592 = ADVANCED_FACE ( 'NONE', ( #1948 ), #22831, .T. ) ;
#21593 = DIRECTION ( 'NONE',  ( 0.000000000000000000, 0.000000000000000000, -1.000000000000000000 ) ) ;
#21594 = ORIENTED_EDGE ( 'NONE', *, *, #2456, .F. ) ;
#21595 = ORIENTED_EDGE ( 'NONE', *, *, #16099, .F. ) ;
#21596 = ORIENTED_EDGE ( 'NONE', *, *, #8742, .T. ) ;
#21597 = CARTESIAN_POINT ( 'NONE',  ( 9.499999999999790390, 3.086737114213260025, 4.159589141758141650 ) ) ;
#21598 = EDGE_CURVE ( 'NONE', #21066, #5168, #11497, .T. ) ;
#21599 = EDGE_CURVE ( 'NONE', #721, #5790, #16194, .T. ) ;
#21600 = AXIS2_PLACEMENT_3D ( 'NONE', #5765, #4185, #15752 ) ;
#21601 = ORIENTED_EDGE ( 'NONE', *, *, #13246, .F. ) ;
#21602 = CARTESIAN_POINT ( 'NONE',  ( 0.000000000000000000, 0.000000000000000000, 0.000000000000000000 ) ) ;
#21603 = VECTOR ( 'NONE', #21542, 1000.000000000000000 ) ;
#21604 = AXIS2_PLACEMENT_3D ( 'NONE', #8574, #12719, #20058 ) ;
#21605 = DIRECTION ( 'NONE',  ( 1.000000000000000000, 0.000000000000000000, -0.000000000000000000 ) ) ;
#21606 = CARTESIAN_POINT ( 'NONE',  ( 9.499999999999799272, 3.086737114213245370, 6.159589141758142539 ) ) ;
#21607 = VECTOR ( 'NONE', #20106, 1000.000000000000000 ) ;
#21608 = CIRCLE ( 'NONE', #7547, 23.84999999999999432 ) ;
#21609 = DIRECTION ( 'NONE',  ( -1.000000000000000000, -1.224606353822377258E-16, -0.000000000000000000 ) ) ;
#21610 = LINE ( 'NONE', #4903, #12929 ) ;
#21611 = CARTESIAN_POINT ( 'NONE',  ( 1.999999999999996669, 45.00000000000000000, -3.000000000000000000 ) ) ;
#21612 = ORIENTED_EDGE ( 'NONE', *, *, #10865, .F. ) ;
#21613 = DIRECTION ( 'NONE',  ( 1.000000000000000000, 0.000000000000000000, 0.000000000000000000 ) ) ;
#21614 = CARTESIAN_POINT ( 'NONE',  ( 7.685661446562381371, -5.583959896777971110, 11.85958914175814449 ) ) ;
#21615 = DIRECTION ( 'NONE',  ( 0.000000000000000000, 0.000000000000000000, -1.000000000000000000 ) ) ;
#21616 = AXIS2_PLACEMENT_3D ( 'NONE', #12064, #1000, #23336 ) ;
#21617 = DIRECTION ( 'NONE',  ( 1.000000000000000000, 0.000000000000000000, 0.000000000000000000 ) ) ;
#21618 = EDGE_LOOP ( 'NONE', ( #3063, #15870, #8438, #7389 ) ) ;
#21619 = SPHERICAL_SURFACE ( 'NONE', #14623, 1.500000000000000000 ) ;
#21620 = ORIENTED_EDGE ( 'NONE', *, *, #11182, .T. ) ;
#21621 = FACE_OUTER_BOUND ( 'NONE', #19350, .T. ) ;
#21622 = AXIS2_PLACEMENT_3D ( 'NONE', #15065, #16668, #9326 ) ;
#21623 = ORIENTED_EDGE ( 'NONE', *, *, #9757, .T. ) ;
#21624 = CARTESIAN_POINT ( 'NONE',  ( -5.365059087798940141, -7.384370330707086261, 3.933165578109187877 ) ) ;
#21625 = EDGE_CURVE ( 'NONE', #3887, #15590, #7671, .T. ) ;
#21626 = DIRECTION ( 'NONE',  ( -0.000000000000000000, -0.000000000000000000, -1.000000000000000000 ) ) ;
#21627 = CARTESIAN_POINT ( 'NONE',  ( -8.000000000000007105, 1.040949779275250534E-15, 0.000000000000000000 ) ) ;
#21628 = CARTESIAN_POINT ( 'NONE',  ( 40.00000000000000000, -28.80990663662251450, 12.00000000000000000 ) ) ;
#21629 = DIRECTION ( 'NONE',  ( -1.000000000000000000, 0.000000000000000000, 0.000000000000000000 ) ) ;
#21630 = LINE ( 'NONE', #15998, #2151 ) ;
#21631 = CIRCLE ( 'NONE', #13423, 5.000000000000007994 ) ;
#21632 = AXIS2_PLACEMENT_3D ( 'NONE', #14802, #64, #14918 ) ;
#21633 = ORIENTED_EDGE ( 'NONE', *, *, #21256, .T. ) ;
#21634 = LINE ( 'NONE', #23708, #9531 ) ;
#21635 = CARTESIAN_POINT ( 'NONE',  ( 7.685661446562381371, -5.583959896777971110, -5.006742014460233037 ) ) ;
#21636 = ORIENTED_EDGE ( 'NONE', *, *, #3030, .F. ) ;
#21637 = AXIS2_PLACEMENT_3D ( 'NONE', #14852, #10941, #22325 ) ;
#21638 = ORIENTED_EDGE ( 'NONE', *, *, #7777, .T. ) ;
#21639 = EDGE_CURVE ( 'NONE', #6803, #19252, #4528, .T. ) ;
#21640 = ORIENTED_EDGE ( 'NONE', *, *, #19235, .F. ) ;
#21641 = DIRECTION ( 'NONE',  ( -0.000000000000000000, -0.000000000000000000, -1.000000000000000000 ) ) ;
#21642 = VECTOR ( 'NONE', #5446, 1000.000000000000000 ) ;
#21643 = AXIS2_PLACEMENT_3D ( 'NONE', #10685, #21454, #1320 ) ;
#21644 = ADVANCED_FACE ( 'NONE', ( #4280 ), #2949, .F. ) ;
#21645 = ORIENTED_EDGE ( 'NONE', *, *, #5081, .T. ) ;
#21646 = DIRECTION ( 'NONE',  ( 0.000000000000000000, 0.000000000000000000, 1.000000000000000000 ) ) ;
#21647 = PLANE ( 'NONE',  #103 ) ;
#21648 = DIRECTION ( 'NONE',  ( -0.000000000000000000, -0.000000000000000000, -1.000000000000000000 ) ) ;
#21649 = ADVANCED_FACE ( 'NONE', ( #13281 ), #13166, .T. ) ;
#21650 = CARTESIAN_POINT ( 'NONE',  ( 84.18181818181818699, 7.491529369508391930E-15, 0.000000000000000000 ) ) ;
#21651 = ORIENTED_EDGE ( 'NONE', *, *, #13159, .F. ) ;
#21652 = DIRECTION ( 'NONE',  ( 0.000000000000000000, 0.000000000000000000, 1.000000000000000000 ) ) ;
#21653 = EDGE_CURVE ( 'NONE', #15898, #23250, #3906, .T. ) ;
#21654 = DIRECTION ( 'NONE',  ( 1.000000000000000000, 0.000000000000000000, 0.000000000000000000 ) ) ;
#21655 = CARTESIAN_POINT ( 'NONE',  ( 1.999999999999994449, -45.00000000000000000, -23.99999999999999645 ) ) ;
#21656 = CIRCLE ( 'NONE', #10391, 50.00000000000000000 ) ;
#21657 = CARTESIAN_POINT ( 'NONE',  ( -1.504652183083727168, 9.499999999999904077, 2.610843423304989308 ) ) ;
#21658 = AXIS2_PLACEMENT_3D ( 'NONE', #20165, #5041, #18089 ) ;
#21659 = VECTOR ( 'NONE', #8363, 1000.000000000000000 ) ;
#21660 = VERTEX_POINT ( 'NONE', #18569 ) ;
#21661 = CIRCLE ( 'NONE', #1396, 5.025000000000002132 ) ;
#21662 = EDGE_LOOP ( 'NONE', ( #22518, #197, #2715, #23115 ) ) ;
#21663 = VERTEX_POINT ( 'NONE', #7783 ) ;
#21664 = CARTESIAN_POINT ( 'NONE',  ( 2.454813078130514813E-15, 16.67999999999999972, 14.50000000000000000 ) ) ;
#21665 = CARTESIAN_POINT ( 'NONE',  ( 1.999999999999996669, -45.00000000000000000, -8.673617379884035472E-16 ) ) ;
#21666 = DIRECTION ( 'NONE',  ( 0.000000000000000000, 0.000000000000000000, 1.000000000000000000 ) ) ;
#21667 = ORIENTED_EDGE ( 'NONE', *, *, #16587, .F. ) ;
#21668 = FACE_OUTER_BOUND ( 'NONE', #23161, .T. ) ;
#21669 = CIRCLE ( 'NONE', #11110, 11.23082370883259706 ) ;
#21670 = CARTESIAN_POINT ( 'NONE',  ( 60.32931906745326245, 7.420530141404717394E-15, 0.000000000000000000 ) ) ;
#21671 = ORIENTED_EDGE ( 'NONE', *, *, #8031, .F. ) ;
#21672 =( GEOMETRIC_REPRESENTATION_CONTEXT ( 3 ) GLOBAL_UNCERTAINTY_ASSIGNED_CONTEXT ( ( #23296 ) ) GLOBAL_UNIT_ASSIGNED_CONTEXT ( ( #19, #13047, #15215 ) ) REPRESENTATION_CONTEXT ( 'NONE', 'WORKASPACE' ) );
#21673 = CARTESIAN_POINT ( 'NONE',  ( 42.00000000000000000, -25.93535998569253920, 27.00000000000000000 ) ) ;
#21674 = CARTESIAN_POINT ( 'NONE',  ( -9.500000000000000000, -6.482511860946779655E-13, 4.206742014460233214 ) ) ;
#21675 = EDGE_CURVE ( 'NONE', #2169, #18707, #18154, .T. ) ;
#21676 = EDGE_CURVE ( 'NONE', #18342, #5783, #12681, .T. ) ;
#21677 = CARTESIAN_POINT ( 'NONE',  ( 0.000000000000000000, -45.00000000000000000, -3.000000000000000000 ) ) ;
#21678 = CIRCLE ( 'NONE', #8009, 5.000000000000007994 ) ;
#21679 = CYLINDRICAL_SURFACE ( 'NONE', #7065, 20.85000000000000142 ) ;
#21680 = VECTOR ( 'NONE', #1894, 1000.000000000000000 ) ;
#21681 = CARTESIAN_POINT ( 'NONE',  ( -14.94777716362147935, -1.291632522116892501, 9.417361603030281358 ) ) ;
#21682 = CARTESIAN_POINT ( 'NONE',  ( -28.99999999999999645, 29.50000000000000711, -3.000000000000000000 ) ) ;
#21683 = CARTESIAN_POINT ( 'NONE',  ( -2.682529543900285862, 8.255977015246234174, -3.233165578109188587 ) ) ;
#21684 = DIRECTION ( 'NONE',  ( -1.000000000000000000, 0.000000000000000000, 0.000000000000000000 ) ) ;
#21685 = ORIENTED_EDGE ( 'NONE', *, *, #4802, .F. ) ;
#21686 = CARTESIAN_POINT ( 'NONE',  ( 8.680847955711007202, 5.912916378492122225E-13, 4.633165578109188942 ) ) ;
#21687 = TOROIDAL_SURFACE ( 'NONE', #1811, 5.999999999999999112, 1.000000000000000000 ) ;
#21688 = PRODUCT_DEFINITION_FORMATION_WITH_SPECIFIED_SOURCE ( 'ANY', '', #9573, .NOT_KNOWN. ) ;
#21689 = CARTESIAN_POINT ( 'NONE',  ( 11.50000000000000000, 17.26667456984545979, 4.623588898214379128 ) ) ;
#21690 = CIRCLE ( 'NONE', #12716, 5.000000000000007994 ) ;
#21691 = EDGE_LOOP ( 'NONE', ( #6575, #2503, #3402, #819 ) ) ;
#21692 = VERTEX_POINT ( 'NONE', #8150 ) ;
#21693 = DIRECTION ( 'NONE',  ( 1.000000000000000000, 0.000000000000000000, 0.000000000000000000 ) ) ;
#21694 = CARTESIAN_POINT ( 'NONE',  ( 7.685661446562381371, -5.583959896777971110, -5.859589141758143604 ) ) ;
#21695 = AXIS2_PLACEMENT_3D ( 'NONE', #20129, #5356, #3405 ) ;
#21696 = EDGE_CURVE ( 'NONE', #5746, #5909, #15481, .T. ) ;
#21697 = CARTESIAN_POINT ( 'NONE',  ( -7.999999999999986677, 0.000000000000000000, 53.00000000000000000 ) ) ;
#21698 = DIRECTION ( 'NONE',  ( 0.000000000000000000, 0.000000000000000000, 1.000000000000000000 ) ) ;
#21699 = DIRECTION ( 'NONE',  ( 0.7071067811865489050, 0.000000000000000000, 0.7071067811865462405 ) ) ;
#21700 = EDGE_CURVE ( 'NONE', #14909, #13595, #15594, .T. ) ;
#21701 = LINE ( 'NONE', #17536, #23876 ) ;
#21702 = ADVANCED_FACE ( 'NONE', ( #22948 ), #15729, .F. ) ;
#21703 = DIRECTION ( 'NONE',  ( 0.000000000000000000, 0.000000000000000000, -1.000000000000000000 ) ) ;
#21704 = EDGE_CURVE ( 'NONE', #11857, #3699, #3342, .T. ) ;
#21705 = EDGE_LOOP ( 'NONE', ( #2716, #848, #5357, #18586 ) ) ;
#21706 = VECTOR ( 'NONE', #13941, 1000.000000000000000 ) ;
#21707 = DIRECTION ( 'NONE',  ( -1.000000000000000000, 0.000000000000000000, 0.000000000000000000 ) ) ;
#21708 = ORIENTED_EDGE ( 'NONE', *, *, #1559, .F. ) ;
#21709 = CYLINDRICAL_SURFACE ( 'NONE', #6732, 1.999999999999994449 ) ;
#21710 = DIRECTION ( 'NONE',  ( 0.000000000000000000, -1.000000000000000000, 0.000000000000000000 ) ) ;
#21711 = DIRECTION ( 'NONE',  ( 0.000000000000000000, 0.000000000000000000, 1.000000000000000000 ) ) ;
#21712 = ORIENTED_EDGE ( 'NONE', *, *, #16064, .F. ) ;
#21713 = DIRECTION ( 'NONE',  ( 0.000000000000000000, 0.000000000000000000, -1.000000000000000000 ) ) ;
#21714 = ORIENTED_EDGE ( 'NONE', *, *, #591, .T. ) ;
#21715 = CARTESIAN_POINT ( 'NONE',  ( 0.000000000000000000, -17.86986844953241516, -0.4282833139928939881 ) ) ;
#21716 = CARTESIAN_POINT ( 'NONE',  ( 7.022953521754877748, 5.102474405760673903, -4.833165578109188232 ) ) ;
#21717 = VERTEX_POINT ( 'NONE', #23434 ) ;
#21718 = ORIENTED_EDGE ( 'NONE', *, *, #11168, .F. ) ;
#21719 = CARTESIAN_POINT ( 'NONE',  ( 6.809999908187194197E-13, -9.988891130263535700, 7.559589141758143782 ) ) ;
#21720 = CARTESIAN_POINT ( 'NONE',  ( -2.935661446561384391, -9.035036904804158553, 6.606742014460233570 ) ) ;
#21721 = EDGE_LOOP ( 'NONE', ( #14886, #13071, #11235, #11622, #13501 ) ) ;
#21722 = CARTESIAN_POINT ( 'NONE',  ( 0.000000000000000000, 0.000000000000000000, 4.000000000000000000 ) ) ;
#21723 = PLANE ( 'NONE',  #10393 ) ;
#21724 = CARTESIAN_POINT ( 'NONE',  ( -5.871322893123449127, -8.081182679344781405, -4.506742014460232149 ) ) ;
#21725 = VERTEX_POINT ( 'NONE', #851 ) ;
#21726 = EDGE_CURVE ( 'NONE', #3425, #18928, #18731, .T. ) ;
#21727 = CARTESIAN_POINT ( 'NONE',  ( 67.60204634018053582, 5.000000000000025757, 6.123233995736788962E-16 ) ) ;
#21728 = FACE_OUTER_BOUND ( 'NONE', #20618, .T. ) ;
#21729 = PRODUCT_DEFINITION_SHAPE ( 'NONE', 'NONE',  #24100 ) ;
#21730 = PLANE ( 'NONE',  #21536 ) ;
#21731 = ORIENTED_EDGE ( 'NONE', *, *, #275, .T. ) ;
#21732 = ADVANCED_FACE ( 'NONE', ( #739 ), #2436, .T. ) ;
#21733 = EDGE_CURVE ( 'NONE', #16728, #1139, #9863, .T. ) ;
#21734 = ORIENTED_EDGE ( 'NONE', *, *, #20214, .F. ) ;
#21735 = CARTESIAN_POINT ( 'NONE',  ( 9.500000000000000000, 6.470877716354879437E-13, 10.05958914175814378 ) ) ;
#21736 = CARTESIAN_POINT ( 'NONE',  ( -31.50000000000000711, -51.00000000000000711, 12.50000000000000000 ) ) ;
#21737 = CARTESIAN_POINT ( 'NONE',  ( -2.466888520469390222, 9.179244532860076689, -3.500783152383143193 ) ) ;
#21738 = PRESENTATION_STYLE_ASSIGNMENT (( #12326 ) ) ;
#21739 = CARTESIAN_POINT ( 'NONE',  ( 76.03431729618309021, -5.000000000000000888, 6.123233995736776143E-16 ) ) ;
#21740 = VERTEX_POINT ( 'NONE', #2569 ) ;
#21741 = CARTESIAN_POINT ( 'NONE',  ( -14.99999999999999822, 0.3242076166095213541, 9.499999999999994671 ) ) ;
#21742 = ORIENTED_EDGE ( 'NONE', *, *, #17819, .T. ) ;
#21743 = CYLINDRICAL_SURFACE ( 'NONE', #13036, 1.000000000000000222 ) ;
#21744 = EDGE_LOOP ( 'NONE', ( #20526, #8945, #12818, #15365 ) ) ;
#21745 = CARTESIAN_POINT ( 'NONE',  ( 8.680847955711199049, -2.820578480813074496, 4.533165578109188409 ) ) ;
#21746 = EDGE_LOOP ( 'NONE', ( #3698, #20303, #9344, #23372 ) ) ;
#21747 = DIRECTION ( 'NONE',  ( -0.000000000000000000, -0.000000000000000000, -1.000000000000000000 ) ) ;
#21748 = SHAPE_REPRESENTATION ( 'MAT-029', ( #7251, #3759, #7635, #14652, #20142, #10369, #13489, #9590, #8023, #6506, #4149, #15038, #8817, #5314, #24014, #2984, #17787, #23265, #267, #19747, #16601, #18949, #4944, #21304 ), #20520 ) ;
#21749 = CARTESIAN_POINT ( 'NONE',  ( 60.90909090909091361, 4.172000000000015696, 0.000000000000000000 ) ) ;
#21750 = CARTESIAN_POINT ( 'NONE',  ( 43.99999999999999289, -51.00000000000000711, 0.000000000000000000 ) ) ;
#21751 = CARTESIAN_POINT ( 'NONE',  ( 40.49999999999998579, 50.99999999999999289, 12.50000000000000000 ) ) ;
#21752 = DIRECTION ( 'NONE',  ( 1.000000000000000000, 0.000000000000000000, 0.000000000000000000 ) ) ;
#21753 = ORIENTED_EDGE ( 'NONE', *, *, #19788, .F. ) ;
#21754 = FACE_OUTER_BOUND ( 'NONE', #16058, .T. ) ;
#21755 = AXIS2_PLACEMENT_3D ( 'NONE', #3583, #9406, #11003 ) ;
#21756 = CARTESIAN_POINT ( 'NONE',  ( -2.935661446562617183, 9.035036904803758873, -7.806742014460233747 ) ) ;
#21757 = ORIENTED_EDGE ( 'NONE', *, *, #712, .F. ) ;
#21758 = ORIENTED_EDGE ( 'NONE', *, *, #18604, .T. ) ;
#21759 = CARTESIAN_POINT ( 'NONE',  ( 63.81818181818181301, 7.491529369508391930E-15, 0.000000000000000000 ) ) ;
#21760 = EDGE_CURVE ( 'NONE', #1139, #20735, #15018, .T. ) ;
#21761 = CARTESIAN_POINT ( 'NONE',  ( 0.000000000000000000, 0.000000000000000000, 15.50000000000000000 ) ) ;
#21762 = DIRECTION ( 'NONE',  ( -1.000000000000000000, -1.224606353822377258E-16, -0.000000000000000000 ) ) ;
#21763 = EDGE_CURVE ( 'NONE', #5954, #11227, #2966, .T. ) ;
#21764 = ORIENTED_EDGE ( 'NONE', *, *, #17199, .T. ) ;
#21765 = LINE ( 'NONE', #1513, #18017 ) ;
#21766 = AXIS2_PLACEMENT_3D ( 'NONE', #20914, #22738, #15143 ) ;
#21767 = DIRECTION ( 'NONE',  ( -1.000000000000000000, -0.000000000000000000, -0.000000000000000000 ) ) ;
#21768 = PLANE ( 'NONE',  #5196 ) ;
#21769 = ORIENTED_EDGE ( 'NONE', *, *, #20610, .F. ) ;
#21770 = CARTESIAN_POINT ( 'NONE',  ( -9.500000000000202505, 3.086737114211975275, -10.10674201446023268 ) ) ;
#21771 = DIRECTION ( 'NONE',  ( 0.000000000000000000, 0.000000000000000000, -1.000000000000000000 ) ) ;
#21772 = CARTESIAN_POINT ( 'NONE',  ( 9.499999999999790390, 3.086737114213260025, -4.159589141758142539 ) ) ;
#21773 = CIRCLE ( 'NONE', #1887, 1.499999999999998002 ) ;
#21774 = CARTESIAN_POINT ( 'NONE',  ( -9.500000000000211386, 3.086737114211961064, 2.959589141758143249 ) ) ;
#21775 = EDGE_LOOP ( 'NONE', ( #542, #1802, #10263, #6289 ) ) ;
#21776 = ADVANCED_FACE ( 'NONE', ( #17320 ), #20125, .F. ) ;
#21777 = ORIENTED_EDGE ( 'NONE', *, *, #10655, .F. ) ;
#21778 = ORIENTED_EDGE ( 'NONE', *, *, #4230, .F. ) ;
#21779 = EDGE_CURVE ( 'NONE', #1599, #11678, #23995, .T. ) ;
#21780 = ORIENTED_EDGE ( 'NONE', *, *, #10912, .T. ) ;
#21781 = DIRECTION ( 'NONE',  ( 0.000000000000000000, 0.5406408174555985546, -0.8412535328311806504 ) ) ;
#21782 = CYLINDRICAL_SURFACE ( 'NONE', #12200, 1.500000000000001332 ) ;
#21783 = ORIENTED_EDGE ( 'NONE', *, *, #11991, .F. ) ;
#21784 = CARTESIAN_POINT ( 'NONE',  ( -12.50000000000000178, 1.672973214995343413E-15, 2.500000000000000000 ) ) ;
#21785 = EDGE_CURVE ( 'NONE', #17838, #16728, #16214, .T. ) ;
#21786 = DIRECTION ( 'NONE',  ( -1.000000000000000000, -1.224606353822377258E-16, -0.000000000000000000 ) ) ;
#21787 = ORIENTED_EDGE ( 'NONE', *, *, #19834, .F. ) ;
#21788 = DIRECTION ( 'NONE',  ( -0.000000000000000000, -0.000000000000000000, 1.000000000000000000 ) ) ;
#21789 = COLOUR_RGB ( '',0.7921568627450980005, 0.8196078431372548767, 0.9333333333333333481 ) ;
#21790 = DIRECTION ( 'NONE',  ( -0.000000000000000000, -0.000000000000000000, -1.000000000000000000 ) ) ;
#21791 = CARTESIAN_POINT ( 'NONE',  ( 0.000000000000000000, 0.000000000000000000, 15.50000000000000000 ) ) ;
#21792 = DIRECTION ( 'NONE',  ( -0.000000000000000000, -0.000000000000000000, -1.000000000000000000 ) ) ;
#21793 = CARTESIAN_POINT ( 'NONE',  ( 74.57977184163763695, 7.562528597612068045E-15, 0.000000000000000000 ) ) ;
#21794 = CARTESIAN_POINT ( 'NONE',  ( 78.36363636363637397, 4.172000000000015696, 5.109226446042767468E-16 ) ) ;
#21795 = CARTESIAN_POINT ( 'NONE',  ( -30.32370777929699202, 42.16181938034195298, -1.500000000000000000 ) ) ;
#21796 = DIRECTION ( 'NONE',  ( 1.000000000000000000, 0.000000000000000000, 0.000000000000000000 ) ) ;
#21797 = ORIENTED_EDGE ( 'NONE', *, *, #15937, .F. ) ;
#21798 = ORIENTED_EDGE ( 'NONE', *, *, #19783, .F. ) ;
#21799 = DIRECTION ( 'NONE',  ( 0.000000000000000000, 0.000000000000000000, -1.000000000000000000 ) ) ;
#21800 = DIRECTION ( 'NONE',  ( 0.000000000000000000, 0.000000000000000000, 1.000000000000000000 ) ) ;
#21801 = ORIENTED_EDGE ( 'NONE', *, *, #1849, .F. ) ;
#21802 = VERTEX_POINT ( 'NONE', #2933 ) ;
#21803 = VECTOR ( 'NONE', #2513, 1000.000000000000000 ) ;
#21804 = EDGE_CURVE ( 'NONE', #1531, #22050, #18551, .T. ) ;
#21805 = DIRECTION ( 'NONE',  ( 0.5735764363510424957, 0.8191520442889943521, 0.000000000000000000 ) ) ;
#21806 = CARTESIAN_POINT ( 'NONE',  ( 6.809999908187194197E-13, -9.988891130263535700, -7.559589141758143782 ) ) ;
#21807 = CARTESIAN_POINT ( 'NONE',  ( -1.514930817284593445, 8.879021050564452011, 101.6186676026875233 ) ) ;
#21808 = LINE ( 'NONE', #9095, #6881 ) ;
#21809 = DIRECTION ( 'NONE',  ( -0.000000000000000000, -0.000000000000000000, -1.000000000000000000 ) ) ;
#21810 = DIRECTION ( 'NONE',  ( -1.000000000000000000, 0.000000000000000000, 0.000000000000000000 ) ) ;
#21811 = ORIENTED_EDGE ( 'NONE', *, *, #12726, .T. ) ;
#21812 = CARTESIAN_POINT ( 'NONE',  ( -41.73082370883257397, 50.99999999999999289, 0.000000000000000000 ) ) ;
#21813 = VECTOR ( 'NONE', #17892, 1000.000000000000114 ) ;
#21814 = VERTEX_POINT ( 'NONE', #23325 ) ;
#21815 = LINE ( 'NONE', #9104, #17609 ) ;
#21816 = ORIENTED_EDGE ( 'NONE', *, *, #22916, .F. ) ;
#21817 = FACE_OUTER_BOUND ( 'NONE', #15189, .T. ) ;
#21818 = LINE ( 'NONE', #17924, #15242 ) ;
#21819 = CARTESIAN_POINT ( 'NONE',  ( 0.000000000000000000, -2.342598717236905603, 4.057500000000010765 ) ) ;
#21820 = DIRECTION ( 'NONE',  ( -0.8571673007021120005, 0.000000000000000000, -0.5150380749100547106 ) ) ;
#21821 = ORIENTED_EDGE ( 'NONE', *, *, #11774, .T. ) ;
#21822 = CARTESIAN_POINT ( 'NONE',  ( -41.00000000000000000, 4.000000000000000888, 10.49999999999999822 ) ) ;
#21823 = CARTESIAN_POINT ( 'NONE',  ( 5.871322893123449127, 8.081182679344781405, -9.506742014460231260 ) ) ;
#21824 = ORIENTED_EDGE ( 'NONE', *, *, #5150, .F. ) ;
#21825 = ORIENTED_EDGE ( 'NONE', *, *, #14838, .F. ) ;
#21826 = CARTESIAN_POINT ( 'NONE',  ( -5.871322893124554021, 8.081182679343978492, 6.759589141758143072 ) ) ;
#21827 = CARTESIAN_POINT ( 'NONE',  ( 2.935661446561383503, 9.035036904804158553, 7.606742014460233570 ) ) ;
#21828 = DIRECTION ( 'NONE',  ( 0.000000000000000000, 0.000000000000000000, -1.000000000000000000 ) ) ;
#21829 = EDGE_LOOP ( 'NONE', ( #10857, #5522, #4687, #8091, #15423 ) ) ;
#21830 = ADVANCED_FACE ( 'NONE', ( #6597 ), #21476, .F. ) ;
#21831 = DIRECTION ( 'NONE',  ( 0.000000000000000000, 0.000000000000000000, 1.000000000000000000 ) ) ;
#21832 = VECTOR ( 'NONE', #10379, 1000.000000000000000 ) ;
#21833 = DIRECTION ( 'NONE',  ( 1.000000000000000000, 0.000000000000000000, 0.000000000000000000 ) ) ;
#21834 = EDGE_CURVE ( 'NONE', #12069, #3216, #13468, .T. ) ;
#21835 = DIRECTION ( 'NONE',  ( -1.000000000000000000, -0.000000000000000000, -0.000000000000000000 ) ) ;
#21836 = CARTESIAN_POINT ( 'NONE',  ( -40.50000000000000711, 50.99999999999999289, 12.50000000000000000 ) ) ;
#21837 = ADVANCED_FACE ( 'NONE', ( #8891 ), #12428, .T. ) ;
#21838 = DIRECTION ( 'NONE',  ( 0.000000000000000000, 0.000000000000000000, 1.000000000000000000 ) ) ;
#21839 = DIRECTION ( 'NONE',  ( -1.000000000000000000, 4.613626265895764052E-16, 0.000000000000000000 ) ) ;
#21840 = ORIENTED_EDGE ( 'NONE', *, *, #17150, .F. ) ;
#21841 = DIRECTION ( 'NONE',  ( 0.000000000000000000, 0.000000000000000000, 1.000000000000000000 ) ) ;
#21842 = CARTESIAN_POINT ( 'NONE',  ( -5.871322893124554021, 8.081182679343978492, 10.75958914175814130 ) ) ;
#21843 = CARTESIAN_POINT ( 'NONE',  ( 78.94340820527399671, 7.562528597612068045E-15, 0.000000000000000000 ) ) ;
#21844 = CARTESIAN_POINT ( 'NONE',  ( 87.09090909090909349, 7.491529369508391930E-15, 0.000000000000000000 ) ) ;
#21845 = CIRCLE ( 'NONE', #17160, 9.500000000000000000 ) ;
#21846 = CARTESIAN_POINT ( 'NONE',  ( 23.00000000000000000, 3.378881074890309311, 11.18737882312122878 ) ) ;
#21847 = CARTESIAN_POINT ( 'NONE',  ( 8.680847955711199049, -2.820578480813074496, -8.533165578109187521 ) ) ;
#21848 = CARTESIAN_POINT ( 'NONE',  ( 0.000000000000000000, 15.23000000000000220, 27.00000000000000000 ) ) ;
#21849 = ORIENTED_EDGE ( 'NONE', *, *, #7102, .F. ) ;
#21850 = EDGE_CURVE ( 'NONE', #7627, #18281, #21285, .T. ) ;
#21851 = CARTESIAN_POINT ( 'NONE',  ( 41.58578643762692195, -26.57671364288190219, 12.00000000000000000 ) ) ;
#21852 = EDGE_LOOP ( 'NONE', ( #9595, #21884, #23311, #1871 ) ) ;
#21853 = CARTESIAN_POINT ( 'NONE',  ( 7.022953521754877748, 5.102474405760673903, 4.833165578109188232 ) ) ;
#21854 = CARTESIAN_POINT ( 'NONE',  ( 60.03431729618309021, 7.562528597612068045E-15, 0.000000000000000000 ) ) ;
#21855 = ORIENTED_EDGE ( 'NONE', *, *, #23042, .F. ) ;
#21856 = CARTESIAN_POINT ( 'NONE',  ( 82.72727272727273373, 7.491529369508391930E-15, 0.000000000000000000 ) ) ;
#21857 = ADVANCED_FACE ( 'NONE', ( #1480 ), #1427, .T. ) ;
#21858 = DIRECTION ( 'NONE',  ( -0.000000000000000000, -0.000000000000000000, -1.000000000000000000 ) ) ;
#21859 = CARTESIAN_POINT ( 'NONE',  ( 2.454813078130514813E-15, 16.67999999999999972, 13.50000000000000178 ) ) ;
#21860 = EDGE_CURVE ( 'NONE', #16259, #19489, #14377, .T. ) ;
#21861 = CARTESIAN_POINT ( 'NONE',  ( 41.99999999999999289, 5.618459588085056979E-15, 0.000000000000000000 ) ) ;
#21862 = EDGE_CURVE ( 'NONE', #19012, #5970, #23248, .T. ) ;
#21863 = ADVANCED_FACE ( 'NONE', ( #22091 ), #16584, .T. ) ;
#21864 = CARTESIAN_POINT ( 'NONE',  ( 71.96568270381689558, 7.420530141404717394E-15, 0.000000000000000000 ) ) ;
#21865 = CARTESIAN_POINT ( 'NONE',  ( 23.85000000000000142, 15.03999999999999915, -27.00000000000000000 ) ) ;
#21866 = CARTESIAN_POINT ( 'NONE',  ( -2.935661446562617183, 9.035036904803758873, -3.806742014460233303 ) ) ;
#21867 = VERTEX_POINT ( 'NONE', #14267 ) ;
#21868 = ORIENTED_EDGE ( 'NONE', *, *, #22568, .F. ) ;
#21869 = CARTESIAN_POINT ( 'NONE',  ( -6.153822176767817416E-13, 9.500000000000000000, -3.500000000000014211 ) ) ;
#21870 = CARTESIAN_POINT ( 'NONE',  ( 41.73082370883260239, 27.62204025492844650, -1.500000000000000000 ) ) ;
#21871 = CARTESIAN_POINT ( 'NONE',  ( 58.57977184163763695, -1.078520768856852078E-29, 5.000000000000007994 ) ) ;
#21872 = LINE ( 'NONE', #2842, #3053 ) ;
#21873 = VERTEX_POINT ( 'NONE', #6954 ) ;
#21874 = DIRECTION ( 'NONE',  ( 1.000000000000000000, 0.000000000000000000, 0.000000000000000000 ) ) ;
#21875 = CARTESIAN_POINT ( 'NONE',  ( 14.51962751333974211, -3.765689428759034563, 8.721787840009190163 ) ) ;
#21876 = ADVANCED_FACE ( 'NONE', ( #12786 ), #6075, .T. ) ;
#21877 = DIRECTION ( 'NONE',  ( -0.000000000000000000, -0.000000000000000000, -1.000000000000000000 ) ) ;
#21878 = CIRCLE ( 'NONE', #7818, 5.000000000000007994 ) ;
#21879 = EDGE_LOOP ( 'NONE', ( #10298, #17785, #5069, #18775 ) ) ;
#21880 = CARTESIAN_POINT ( 'NONE',  ( -5.871322893124554021, 8.081182679343978492, -9.906742014460235168 ) ) ;
#21881 = LINE ( 'NONE', #4949, #17623 ) ;
#21882 = AXIS2_PLACEMENT_3D ( 'NONE', #11160, #20228, #1804 ) ;
#21883 = CARTESIAN_POINT ( 'NONE',  ( -5.871322893124554021, 8.081182679343978492, 2.759589141758142627 ) ) ;
#21884 = ORIENTED_EDGE ( 'NONE', *, *, #4700, .T. ) ;
#21885 = EDGE_CURVE ( 'NONE', #1372, #1207, #3782, .T. ) ;
#21886 = VERTEX_POINT ( 'NONE', #4898 ) ;
#21887 = ORIENTED_EDGE ( 'NONE', *, *, #16121, .T. ) ;
#21888 = CARTESIAN_POINT ( 'NONE',  ( -41.00000000000000000, -5.000000000000000888, 9.500000000000000000 ) ) ;
#21889 = LINE ( 'NONE', #1848, #21977 ) ;
#21890 = CYLINDRICAL_SURFACE ( 'NONE', #7137, 11.22592346138681130 ) ;
#21891 = EDGE_LOOP ( 'NONE', ( #8649, #18885, #3464, #22336, #15386 ) ) ;
#21892 = ORIENTED_EDGE ( 'NONE', *, *, #2690, .T. ) ;
#21893 = DIRECTION ( 'NONE',  ( -1.000000000000000000, -1.224606353822377258E-16, -0.000000000000000000 ) ) ;
#21894 = CIRCLE ( 'NONE', #858, 10.00000000000000178 ) ;
#21895 = ORIENTED_EDGE ( 'NONE', *, *, #8347, .T. ) ;
#21896 = CARTESIAN_POINT ( 'NONE',  ( -6.153822176767817416E-13, 9.500000000000000000, -3.706742014460231882 ) ) ;
#21897 = CARTESIAN_POINT ( 'NONE',  ( 0.000000000000000000, 0.000000000000000000, 0.000000000000000000 ) ) ;
#21898 = CARTESIAN_POINT ( 'NONE',  ( 5.871322893124553133, -8.081182679343980269, 4.906742014460232504 ) ) ;
#21899 = PLANE ( 'NONE',  #14776 ) ;
#21900 = CARTESIAN_POINT ( 'NONE',  ( 40.00000000000000000, 0.000000000000000000, 11.00000000000000000 ) ) ;
#21901 = CARTESIAN_POINT ( 'NONE',  ( -41.51716637648671338, 25.94562225875360539, 12.00000000000000000 ) ) ;
#21902 = CARTESIAN_POINT ( 'NONE',  ( -6.250000000000000888, 10.82531754730548279, 2.500000000000000000 ) ) ;
#21903 = EDGE_CURVE ( 'NONE', #1819, #13107, #14638, .T. ) ;
#21904 = DIRECTION ( 'NONE',  ( -5.501724186093585079E-16, -1.000000000000000000, 0.000000000000000000 ) ) ;
#21905 = CARTESIAN_POINT ( 'NONE',  ( -14.99999999999999467, 0.3238088414458165643, -9.499999999999996447 ) ) ;
#21906 = CARTESIAN_POINT ( 'NONE',  ( -2.682529543899159208, -8.255977015246598327, 12.03316557810918930 ) ) ;
#21907 = ORIENTED_EDGE ( 'NONE', *, *, #20537, .F. ) ;
#21908 = CIRCLE ( 'NONE', #3980, 9.000000000000000000 ) ;
#21909 = VECTOR ( 'NONE', #23789, 1000.000000000000000 ) ;
#21910 = CIRCLE ( 'NONE', #12154, 8.000000000000003553 ) ;
#21911 = AXIS2_PLACEMENT_3D ( 'NONE', #21589, #15847, #1209 ) ;
#21912 = EDGE_CURVE ( 'NONE', #14761, #18444, #21955, .T. ) ;
#21913 = PRODUCT_DEFINITION_SHAPE ( 'NONE', 'NONE',  #8241 ) ;
#21914 = AXIS2_PLACEMENT_3D ( 'NONE', #23367, #17480, #8568 ) ;
#21915 = DIRECTION ( 'NONE',  ( 0.9596546673583324916, 0.2811812927941123030, -5.551115123125782702E-17 ) ) ;
#21916 = CIRCLE ( 'NONE', #12541, 1.500000000000001332 ) ;
#21917 = DIRECTION ( 'NONE',  ( 0.000000000000000000, 0.000000000000000000, 1.000000000000000000 ) ) ;
#21918 = ORIENTED_EDGE ( 'NONE', *, *, #15418, .T. ) ;
#21919 = ORIENTED_EDGE ( 'NONE', *, *, #7798, .T. ) ;
#21920 = CARTESIAN_POINT ( 'NONE',  ( 5.000000000000000000, 4.685197434473818312, -1.301042606982605321E-15 ) ) ;
#21921 = CARTESIAN_POINT ( 'NONE',  ( 9.500000000000209610, -3.086737114211962396, -3.959589141758145026 ) ) ;
#21922 = CYLINDRICAL_SURFACE ( 'NONE', #7926, 5.000000000000000888 ) ;
#21923 = FACE_OUTER_BOUND ( 'NONE', #11336, .T. ) ;
#21924 = PLANE ( 'NONE',  #3710 ) ;
#21925 = DIRECTION ( 'NONE',  ( -4.625929269271481378E-15, 1.000000000000000000, 0.000000000000000000 ) ) ;
#21926 = ORIENTED_EDGE ( 'NONE', *, *, #23492, .T. ) ;
#21927 = DIRECTION ( 'NONE',  ( 0.000000000000000000, 0.000000000000000000, 1.000000000000000000 ) ) ;
#21928 = AXIS2_PLACEMENT_3D ( 'NONE', #19866, #1204, #23532 ) ;
#21929 = AXIS2_PLACEMENT_3D ( 'NONE', #13052, #20513, #22470 ) ;
#21930 = AXIS2_PLACEMENT_3D ( 'NONE', #18904, #7, #22560 ) ;
#21931 = EDGE_CURVE ( 'NONE', #18942, #20443, #11112, .T. ) ;
#21932 = CARTESIAN_POINT ( 'NONE',  ( -20.84999999999999787, -16.67999999999985050, 13.50000000000000178 ) ) ;
#21933 = VERTEX_POINT ( 'NONE', #21836 ) ;
#21934 = DIRECTION ( 'NONE',  ( -1.000000000000000000, 0.000000000000000000, 0.000000000000000000 ) ) ;
#21935 = VECTOR ( 'NONE', #9472, 1000.000000000000000 ) ;
#21936 = DIRECTION ( 'NONE',  ( -0.5735764363510519326, 0.8191520442889876907, 1.003171929053519816E-16 ) ) ;
#21937 = PLANE ( 'NONE',  #23940 ) ;
#21938 = AXIS2_PLACEMENT_3D ( 'NONE', #8050, #21115, #2589 ) ;
#21939 = DIRECTION ( 'NONE',  ( -0.000000000000000000, -0.000000000000000000, -1.000000000000000000 ) ) ;
#21940 = EDGE_CURVE ( 'NONE', #11642, #1246, #10828, .T. ) ;
#21941 = ORIENTED_EDGE ( 'NONE', *, *, #7886, .F. ) ;
#21942 = FACE_OUTER_BOUND ( 'NONE', #18597, .T. ) ;
#21943 = AXIS2_PLACEMENT_3D ( 'NONE', #1606, #18091, #23707 ) ;
#21944 = DIRECTION ( 'NONE',  ( 0.000000000000000000, 0.000000000000000000, 1.000000000000000000 ) ) ;
#21945 = ORIENTED_EDGE ( 'NONE', *, *, #18882, .F. ) ;
#21946 = EDGE_CURVE ( 'NONE', #11259, #21867, #1579, .T. ) ;
#21947 = ORIENTED_EDGE ( 'NONE', *, *, #4738, .F. ) ;
#21948 = CARTESIAN_POINT ( 'NONE',  ( 7.685661446561619314, 5.583959896779020049, 11.40674201446023517 ) ) ;
#21949 = CARTESIAN_POINT ( 'NONE',  ( 5.871322893124553133, -8.081182679343980269, 6.906742014460234280 ) ) ;
#21950 = ORIENTED_EDGE ( 'NONE', *, *, #10682, .T. ) ;
#21951 = ORIENTED_EDGE ( 'NONE', *, *, #1516, .F. ) ;
#21952 = DIRECTION ( 'NONE',  ( 0.000000000000000000, 0.000000000000000000, 1.000000000000000000 ) ) ;
#21953 = CIRCLE ( 'NONE', #11393, 6.050000000006050982 ) ;
#21954 = VECTOR ( 'NONE', #11271, 1000.000000000000000 ) ;
#21955 = LINE ( 'NONE', #5242, #22079 ) ;
#21956 = AXIS2_PLACEMENT_3D ( 'NONE', #926, #8350, #17760 ) ;
#21957 = CIRCLE ( 'NONE', #4438, 4.172000000000008590 ) ;
#21958 = VECTOR ( 'NONE', #4053, 1000.000000000000000 ) ;
#21959 = LINE ( 'NONE', #18191, #22710 ) ;
#21960 = CIRCLE ( 'NONE', #18455, 14.72592346043842326 ) ;
#21961 = CARTESIAN_POINT ( 'NONE',  ( -7.685661446562381371, 5.583959896777970222, -10.85958914175814449 ) ) ;
#21962 = VERTEX_POINT ( 'NONE', #7181 ) ;
#21963 = DIRECTION ( 'NONE',  ( -0.000000000000000000, -0.000000000000000000, -1.000000000000000000 ) ) ;
#21964 = DIRECTION ( 'NONE',  ( -0.000000000000000000, -0.000000000000000000, 1.000000000000000000 ) ) ;
#21965 = CARTESIAN_POINT ( 'NONE',  ( -2.024999999999999911, -45.00000000000000000, -3.000000000000000000 ) ) ;
#21966 = CARTESIAN_POINT ( 'NONE',  ( -6.944120675781903174, 6.490472247601844380, -3.501262065910452748 ) ) ;
#21967 = CARTESIAN_POINT ( 'NONE',  ( 2.935661446562616295, -9.035036904803758873, -11.65958914175814520 ) ) ;
#21968 = VECTOR ( 'NONE', #9740, 1000.000000000000000 ) ;
#21969 = CYLINDRICAL_SURFACE ( 'NONE', #1577, 0.9999999999999991118 ) ;
#21970 = EDGE_CURVE ( 'NONE', #678, #21154, #14621, .T. ) ;
#21971 = EDGE_CURVE ( 'NONE', #17223, #12845, #2172, .T. ) ;
#21972 = AXIS2_PLACEMENT_3D ( 'NONE', #10864, #18334, #16495 ) ;
#21973 = CARTESIAN_POINT ( 'NONE',  ( -1.999999999999994449, -45.00000000000000000, 3.000000000000002665 ) ) ;
#21974 = AXIS2_PLACEMENT_3D ( 'NONE', #2491, #11731, #9776 ) ;
#21975 = VERTEX_POINT ( 'NONE', #19015 ) ;
#21976 = DIRECTION ( 'NONE',  ( -1.000000000000000000, 0.000000000000000000, 0.000000000000000000 ) ) ;
#21977 = VECTOR ( 'NONE', #6775, 1000.000000000000000 ) ;
#21978 = VERTEX_POINT ( 'NONE', #7517 ) ;
#21979 = CARTESIAN_POINT ( 'NONE',  ( -9.500000000000000000, -6.482511860946779655E-13, -9.059589141758143782 ) ) ;
#21980 = AXIS2_PLACEMENT_3D ( 'NONE', #10059, #15677, #17513 ) ;
#21981 = CARTESIAN_POINT ( 'NONE',  ( -6.249999999999999112, -10.82531754730548279, -2.500000000000000000 ) ) ;
#21982 = AXIS2_PLACEMENT_3D ( 'NONE', #18990, #6279, #13606 ) ;
#21983 = ORIENTED_EDGE ( 'NONE', *, *, #6830, .F. ) ;
#21984 = CARTESIAN_POINT ( 'NONE',  ( 14.51962751333974389, -3.765689428759035895, 27.00000000000000000 ) ) ;
#21985 = CARTESIAN_POINT ( 'NONE',  ( 0.000000000000000000, 0.000000000000000000, 0.000000000000000000 ) ) ;
#21986 = AXIS2_PLACEMENT_3D ( 'NONE', #8137, #15582, #13906 ) ;
#21987 = CARTESIAN_POINT ( 'NONE',  ( 73.42022815836234884, -5.000000000000009770, 0.000000000000000000 ) ) ;
#21988 = ORIENTED_EDGE ( 'NONE', *, *, #6153, .F. ) ;
#21989 = CARTESIAN_POINT ( 'NONE',  ( 41.58578643762692195, 26.57671364288191285, 12.00000000000000000 ) ) ;
#21990 = LINE ( 'NONE', #20967, #9177 ) ;
#21991 = AXIS2_PLACEMENT_3D ( 'NONE', #14389, #7192, #5376 ) ;
#21992 = ADVANCED_FACE ( 'NONE', ( #5476 ), #15831, .F. ) ;
#21993 = CARTESIAN_POINT ( 'NONE',  ( -7.685661446562381371, 5.583959896777970222, -6.006742014460233037 ) ) ;
#21994 = ORIENTED_EDGE ( 'NONE', *, *, #19024, .F. ) ;
#21995 = CIRCLE ( 'NONE', #20429, 5.100000000000000533 ) ;
#21996 = ORIENTED_EDGE ( 'NONE', *, *, #10656, .F. ) ;
#21997 = CARTESIAN_POINT ( 'NONE',  ( -39.99999999999999289, 27.79189783386526358, 27.00000000000000000 ) ) ;
#21998 = CARTESIAN_POINT ( 'NONE',  ( -29.00000000000000000, -29.49999999999999645, 11.50000000000000000 ) ) ;
#21999 = AXIS2_PLACEMENT_3D ( 'NONE', #20766, #13072, #1864 ) ;
#22000 = AXIS2_PLACEMENT_3D ( 'NONE', #22153, #21786, #5424 ) ;
#22001 = DIRECTION ( 'NONE',  ( -0.000000000000000000, -0.000000000000000000, -1.000000000000000000 ) ) ;
#22002 = CARTESIAN_POINT ( 'NONE',  ( 0.000000000000000000, 0.000000000000000000, 0.000000000000000000 ) ) ;
#22003 = EDGE_CURVE ( 'NONE', #1898, #11303, #22663, .T. ) ;
#22004 = CIRCLE ( 'NONE', #4491, 1.000000000000000888 ) ;
#22005 = EDGE_CURVE ( 'NONE', #7419, #13357, #17770, .T. ) ;
#22006 = VERTEX_POINT ( 'NONE', #12899 ) ;
#22007 = ADVANCED_FACE ( 'NONE', ( #5946 ), #2289, .T. ) ;
#22008 = DIRECTION ( 'NONE',  ( -1.000000000000000000, -0.000000000000000000, -0.000000000000000000 ) ) ;
#22009 = CARTESIAN_POINT ( 'NONE',  ( 14.79187224938325151, -2.570168443617190324, 9.168425918763418281 ) ) ;
#22010 = DIRECTION ( 'NONE',  ( -1.000000000000000000, 0.000000000000000000, 0.000000000000000000 ) ) ;
#22011 = EDGE_LOOP ( 'NONE', ( #7442, #6045, #3447, #12809 ) ) ;
#22012 = CARTESIAN_POINT ( 'NONE',  ( 31.10231664966676846, -45.36128193761570770, 11.00000000000000000 ) ) ;
#22013 = DIRECTION ( 'NONE',  ( 0.000000000000000000, 0.000000000000000000, 1.000000000000000000 ) ) ;
#22014 = CARTESIAN_POINT ( 'NONE',  ( -9.500000000000211386, 3.086737114211961064, -4.106742014460232681 ) ) ;
#22015 = CARTESIAN_POINT ( 'NONE',  ( -31.74999999999995737, 0.000000000000000000, 0.000000000000000000 ) ) ;
#22016 = CIRCLE ( 'NONE', #18116, 9.499999999999998224 ) ;
#22017 = ORIENTED_EDGE ( 'NONE', *, *, #18604, .F. ) ;
#22018 = VECTOR ( 'NONE', #13133, 1000.000000000000000 ) ;
#22019 = EDGE_LOOP ( 'NONE', ( #24019, #6536, #2327, #130, #5655 ) ) ;
#22020 = CIRCLE ( 'NONE', #14596, 18.49999999999999645 ) ;
#22021 = ORIENTED_EDGE ( 'NONE', *, *, #6276, .F. ) ;
#22022 = EDGE_LOOP ( 'NONE', ( #22762, #18672, #15783, #22232 ) ) ;
#22023 = LINE ( 'NONE', #8937, #269 ) ;
#22024 = AXIS2_PLACEMENT_3D ( 'NONE', #19752, #6568, #17792 ) ;
#22025 = EDGE_CURVE ( 'NONE', #18771, #18651, #21083, .T. ) ;
#22026 = DIRECTION ( 'NONE',  ( -0.7071067811865444641, 0.000000000000000000, -0.7071067811865505703 ) ) ;
#22027 = VERTEX_POINT ( 'NONE', #14846 ) ;
#22028 = EDGE_LOOP ( 'NONE', ( #23894, #17676 ) ) ;
#22029 = CARTESIAN_POINT ( 'NONE',  ( 58.57977184163763695, 7.562528597612068045E-15, 0.000000000000000000 ) ) ;
#22030 = ORIENTED_EDGE ( 'NONE', *, *, #22910, .T. ) ;
#22031 =( BOUNDED_CURVE ( )  B_SPLINE_CURVE ( 3, ( #6539, #21989, #14293, #799 ),
 .UNSPECIFIED., .F., .F. ) 
 B_SPLINE_CURVE_WITH_KNOTS ( ( 4, 4 ),
 ( 1.570796326794896558, 3.141592653589793116 ),
 .UNSPECIFIED. ) 
 CURVE ( )  GEOMETRIC_REPRESENTATION_ITEM ( )  RATIONAL_B_SPLINE_CURVE ( ( 1.000000000000000000, 0.8047378541243649375, 0.8047378541243649375, 1.000000000000000000 ) ) 
 REPRESENTATION_ITEM ( '' )  );
#22032 = DIRECTION ( 'NONE',  ( 1.000000000000000000, 0.000000000000000000, 0.000000000000000000 ) ) ;
#22033 = CARTESIAN_POINT ( 'NONE',  ( -9.319542265568680151, 1.279802608863929159, 12.09643368198983104 ) ) ;
#22034 = EDGE_CURVE ( 'NONE', #15534, #12989, #20884, .T. ) ;
#22035 = DIRECTION ( 'NONE',  ( 0.000000000000000000, 0.000000000000000000, 1.000000000000000000 ) ) ;
#22036 = ADVANCED_FACE ( 'NONE', ( #13386 ), #22315, .T. ) ;
#22037 = CARTESIAN_POINT ( 'NONE',  ( -5.871322893123449127, -8.081182679344781405, 10.50674201446023304 ) ) ;
#22038 = FACE_OUTER_BOUND ( 'NONE', #7940, .T. ) ;
#22039 = AXIS2_PLACEMENT_3D ( 'NONE', #16985, #296, #3824 ) ;
#22040 = DIRECTION ( 'NONE',  ( 1.000000000000000000, 1.224606353822377258E-16, 0.000000000000000000 ) ) ;
#22041 = AXIS2_PLACEMENT_3D ( 'NONE', #9369, #16820, #13549 ) ;
#22042 = DIRECTION ( 'NONE',  ( -1.000000000000000000, -0.000000000000000000, -0.000000000000000000 ) ) ;
#22043 = CARTESIAN_POINT ( 'NONE',  ( -31.74999999999995737, 0.000000000000000000, 0.000000000000000000 ) ) ;
#22044 = LINE ( 'NONE', #3725, #12686 ) ;
#22045 = CIRCLE ( 'NONE', #1412, 8.000000000000000000 ) ;
#22046 = CIRCLE ( 'NONE', #1006, 11.68650000001168898 ) ;
#22047 = VERTEX_POINT ( 'NONE', #459 ) ;
#22048 = CARTESIAN_POINT ( 'NONE',  ( 7.022953521755574080, -5.102474405759714671, 12.43316557810918788 ) ) ;
#22049 = AXIS2_PLACEMENT_3D ( 'NONE', #14007, #1090, #8615 ) ;
#22050 = VERTEX_POINT ( 'NONE', #13255 ) ;
#22051 = ITEM_DEFINED_TRANSFORMATION ( 'NONE', 'NONE', #7635,  #17768 ) ;
#22052 = CARTESIAN_POINT ( 'NONE',  ( 74.57977184163763695, 7.562528597612068045E-15, 0.000000000000000000 ) ) ;
#22053 = ORIENTED_EDGE ( 'NONE', *, *, #843, .T. ) ;
#22054 = ORIENTED_EDGE ( 'NONE', *, *, #8671, .T. ) ;
#22055 = CARTESIAN_POINT ( 'NONE',  ( 0.000000000000000000, 0.000000000000000000, 0.000000000000000000 ) ) ;
#22056 = CARTESIAN_POINT ( 'NONE',  ( -2.935661446562617183, 9.035036904803758873, -8.659589141758143427 ) ) ;
#22057 = CIRCLE ( 'NONE', #2574, 1.000000000000000888 ) ;
#22058 = AXIS2_PLACEMENT_3D ( 'NONE', #12922, #5624, #7667 ) ;
#22059 = VECTOR ( 'NONE', #7909, 1000.000000000000000 ) ;
#22060 = FACE_OUTER_BOUND ( 'NONE', #20217, .T. ) ;
#22061 = CARTESIAN_POINT ( 'NONE',  ( -5.976739099259236459E-13, 9.226949318570335734, 3.515549869009883643 ) ) ;
#22062 = FACE_OUTER_BOUND ( 'NONE', #16029, .T. ) ;
#22063 = B_SPLINE_CURVE_WITH_KNOTS ( 'NONE', 3,
 ( #19057, #16521, #22702, #2330, #22033, #4292, #7921, #15371, #14566, #5316, #11695, #2446, #23973, #3917 ),
 .UNSPECIFIED., .F., .F.,
 ( 4, 2, 2, 2, 2, 2, 4 ),
 ( 0.01861151281497951115, 0.01937988632622441448, 0.02014825983746932128, 0.02168500685995913141, 0.02245338037120403474, 0.02322175388244893807, 0.02475850090493875166 ),
 .UNSPECIFIED. ) ;
#22064 = AXIS2_PLACEMENT_3D ( 'NONE', #23274, #10536, #19728 ) ;
#22065 = DIRECTION ( 'NONE',  ( -0.000000000000000000, -0.000000000000000000, 1.000000000000000000 ) ) ;
#22066 = VERTEX_POINT ( 'NONE', #20711 ) ;
#22067 = CARTESIAN_POINT ( 'NONE',  ( 2.935661446562616295, -9.035036904803758873, -6.806742014460233747 ) ) ;
#22068 = ORIENTED_EDGE ( 'NONE', *, *, #1754, .F. ) ;
#22069 = CARTESIAN_POINT ( 'NONE',  ( 0.000000000000000000, -15.03999999999999915, 25.00000000000000000 ) ) ;
#22070 = EDGE_CURVE ( 'NONE', #14785, #17477, #18175, .T. ) ;
#22071 = DIRECTION ( 'NONE',  ( 1.000000000000000000, 0.000000000000000000, 0.000000000000000000 ) ) ;
#22072 = DIRECTION ( 'NONE',  ( -1.000000000000000000, -1.224606353822377258E-16, -0.000000000000000000 ) ) ;
#22073 = FACE_OUTER_BOUND ( 'NONE', #7002, .T. ) ;
#22074 = CARTESIAN_POINT ( 'NONE',  ( -20.84999999999999787, 16.67999999999985405, 13.00000000000000178 ) ) ;
#22075 = CIRCLE ( 'NONE', #10367, 6.050000000006050982 ) ;
#22076 = PRODUCT_DEFINITION_FORMATION_WITH_SPECIFIED_SOURCE ( 'ANY', '', #857, .NOT_KNOWN. ) ;
#22077 = DIRECTION ( 'NONE',  ( -0.000000000000000000, 0.000000000000000000, 1.000000000000000000 ) ) ;
#22078 = ORIENTED_EDGE ( 'NONE', *, *, #1443, .T. ) ;
#22079 = VECTOR ( 'NONE', #16225, 1000.000000000000000 ) ;
#22080 = ORIENTED_EDGE ( 'NONE', *, *, #19250, .F. ) ;
#22081 = CARTESIAN_POINT ( 'NONE',  ( -9.499999999999790390, -3.086737114213257804, 8.306742014460233747 ) ) ;
#22082 = CARTESIAN_POINT ( 'NONE',  ( -7.685661446562381371, 5.583959896777970222, 8.006742014460233037 ) ) ;
#22083 = FACE_OUTER_BOUND ( 'NONE', #11395, .T. ) ;
#22084 = ORIENTED_EDGE ( 'NONE', *, *, #6585, .F. ) ;
#22085 = ORIENTED_EDGE ( 'NONE', *, *, #12855, .F. ) ;
#22086 =( LENGTH_UNIT ( ) NAMED_UNIT ( * ) SI_UNIT ( .MILLI., .METRE. ) );
#22087 = AXIS2_PLACEMENT_3D ( 'NONE', #8886, #23547, #6949 ) ;
#22088 = CARTESIAN_POINT ( 'NONE',  ( -20.84999999999999787, 16.67999999999985405, 14.50000000000000000 ) ) ;
#22089 = CARTESIAN_POINT ( 'NONE',  ( 4.489900896931573904, 0.000000000000000000, 0.000000000000000000 ) ) ;
#22090 = DIRECTION ( 'NONE',  ( -0.000000000000000000, -0.000000000000000000, 1.000000000000000000 ) ) ;
#22091 = FACE_OUTER_BOUND ( 'NONE', #11158, .T. ) ;
#22092 = ADVANCED_FACE ( 'NONE', ( #18653 ), #1928, .T. ) ;
#22093 = DIRECTION ( 'NONE',  ( 0.000000000000000000, -1.000000000000000000, 0.000000000000000000 ) ) ;
#22094 = CARTESIAN_POINT ( 'NONE',  ( 0.000000000000000000, 0.000000000000000000, 3.499999999999999556 ) ) ;
#22095 = DIRECTION ( 'NONE',  ( -0.000000000000000000, -0.000000000000000000, -1.000000000000000000 ) ) ;
#22096 = EDGE_CURVE ( 'NONE', #15497, #21717, #344, .T. ) ;
#22097 = CIRCLE ( 'NONE', #22870, 5.000000000000007994 ) ;
#22099 = EDGE_CURVE ( 'NONE', #11227, #16017, #20497, .T. ) ;
#22098 = DIRECTION ( 'NONE',  ( -1.000000000000000000, 0.000000000000000000, 0.000000000000000000 ) ) ;
#22100 = ORIENTED_EDGE ( 'NONE', *, *, #10790, .T. ) ;
#22101 = AXIS2_PLACEMENT_3D ( 'NONE', #19833, #14316, #21781 ) ;
#22102 = EDGE_CURVE ( 'NONE', #23824, #8454, #7758, .T. ) ;
#22103 = DIRECTION ( 'NONE',  ( -0.000000000000000000, -0.000000000000000000, 1.000000000000000000 ) ) ;
#22104 = ORIENTED_EDGE ( 'NONE', *, *, #20665, .F. ) ;
#22105 = CARTESIAN_POINT ( 'NONE',  ( 5.000000000000000000, -2.342598717236905603, 4.057500000000010765 ) ) ;
#22106 = DIRECTION ( 'NONE',  ( -0.000000000000000000, -0.000000000000000000, -1.000000000000000000 ) ) ;
#22107 = CARTESIAN_POINT ( 'NONE',  ( 0.000000000000000000, 0.000000000000000000, 11.00000000000000000 ) ) ;
#22108 = DIRECTION ( 'NONE',  ( 0.000000000000000000, 0.000000000000000000, 1.000000000000000000 ) ) ;
#22109 = CIRCLE ( 'NONE', #3381, 5.000000000000007994 ) ;
#22110 = DIRECTION ( 'NONE',  ( 0.000000000000000000, 0.000000000000000000, 1.000000000000000000 ) ) ;
#22111 = CIRCLE ( 'NONE', #15857, 14.02592346138681201 ) ;
#22112 = CARTESIAN_POINT ( 'NONE',  ( 9.499999999999790390, 3.086737114213260025, 8.159589141758143427 ) ) ;
#22113 = ORIENTED_EDGE ( 'NONE', *, *, #13816, .T. ) ;
#22114 = DIRECTION ( 'NONE',  ( 0.000000000000000000, -1.000000000000000000, 0.000000000000000000 ) ) ;
#22115 = ORIENTED_EDGE ( 'NONE', *, *, #22961, .F. ) ;
#22116 = CARTESIAN_POINT ( 'NONE',  ( 82.14750088563508257, 7.420530141404717394E-15, 0.000000000000000000 ) ) ;
#22117 = TOROIDAL_SURFACE ( 'NONE', #13919, 3.999999999999999112, 1.000000000000000000 ) ;
#22118 = VERTEX_POINT ( 'NONE', #11912 ) ;
#22119 = PLANE ( 'NONE',  #10770 ) ;
#22120 = AXIS2_PLACEMENT_3D ( 'NONE', #19020, #2293, #4512 ) ;
#22121 = FACE_OUTER_BOUND ( 'NONE', #3787, .T. ) ;
#22122 = CARTESIAN_POINT ( 'NONE',  ( -6.153822176767817416E-13, 9.500000000000000000, -2.559589141758142894 ) ) ;
#22123 = CARTESIAN_POINT ( 'NONE',  ( 29.00000000000000000, 29.50000000000000355, 11.50000000000000000 ) ) ;
#22124 = CARTESIAN_POINT ( 'NONE',  ( 35.99999999999999289, 50.99999999999999289, 0.5000000000000000000 ) ) ;
#22125 = EDGE_CURVE ( 'NONE', #12983, #128, #7615, .T. ) ;
#22126 = EDGE_CURVE ( 'NONE', #16165, #5560, #955, .T. ) ;
#22127 = CARTESIAN_POINT ( 'NONE',  ( 5.871322893124553133, -8.081182679343980269, -7.759589141758143072 ) ) ;
#22128 = ORIENTED_EDGE ( 'NONE', *, *, #4058, .T. ) ;
#22129 = VERTEX_POINT ( 'NONE', #17287 ) ;
#22130 = DIRECTION ( 'NONE',  ( -0.000000000000000000, -0.000000000000000000, -1.000000000000000000 ) ) ;
#22131 = DIRECTION ( 'NONE',  ( 0.000000000000000000, 0.000000000000000000, 1.000000000000000000 ) ) ;
#22132 = ORIENTED_EDGE ( 'NONE', *, *, #13363, .F. ) ;
#22133 = LINE ( 'NONE', #16970, #21142 ) ;
#22134 = DIRECTION ( 'NONE',  ( -0.000000000000000000, -0.000000000000000000, -1.000000000000000000 ) ) ;
#22135 = EDGE_LOOP ( 'NONE', ( #257, #9316, #17929, #22755, #6904 ) ) ;
#22136 = CARTESIAN_POINT ( 'NONE',  ( 72.54545454545454675, 7.491529369508391930E-15, 0.000000000000000000 ) ) ;
#22137 = LINE ( 'NONE', #3692, #8669 ) ;
#22138 = DIRECTION ( 'NONE',  ( 0.000000000000000000, -0.5406408174555870083, -0.8412535328311879779 ) ) ;
#22139 = EDGE_CURVE ( 'NONE', #3902, #3687, #6484, .T. ) ;
#22140 = CARTESIAN_POINT ( 'NONE',  ( -8.680847955711200825, 2.820578480813073607, 3.533165578109187965 ) ) ;
#22141 = VERTEX_POINT ( 'NONE', #6448 ) ;
#22142 = CIRCLE ( 'NONE', #8489, 1.000000000000000888 ) ;
#22143 = EDGE_CURVE ( 'NONE', #3047, #8203, #13892, .T. ) ;
#22144 = CIRCLE ( 'NONE', #14333, 15.00000000000000000 ) ;
#22145 = ORIENTED_EDGE ( 'NONE', *, *, #13219, .F. ) ;
#22146 = EDGE_CURVE ( 'NONE', #12203, #12368, #14274, .T. ) ;
#22147 = EDGE_LOOP ( 'NONE', ( #8983, #3667, #2973, #23865 ) ) ;
#22148 = PLANE ( 'NONE',  #13449 ) ;
#22149 = EDGE_CURVE ( 'NONE', #23700, #5821, #20521, .T. ) ;
#22150 = FACE_OUTER_BOUND ( 'NONE', #11134, .T. ) ;
#22151 = ORIENTED_EDGE ( 'NONE', *, *, #11828, .F. ) ;
#22152 = VERTEX_POINT ( 'NONE', #10074 ) ;
#22153 = CARTESIAN_POINT ( 'NONE',  ( 65.27272727272728048, 7.491529369508391930E-15, 0.000000000000000000 ) ) ;
#22154 = EDGE_LOOP ( 'NONE', ( #20295, #4668 ) ) ;
#22155 = DIRECTION ( 'NONE',  ( 0.000000000000000000, 0.2817325568414236758, 0.9594929736144991450 ) ) ;
#22156 = FACE_BOUND ( 'NONE', #15619, .T. ) ;
#22157 = CARTESIAN_POINT ( 'NONE',  ( 9.500000000000000000, 6.470877716354879437E-13, 11.20674201446023410 ) ) ;
#22158 = CIRCLE ( 'NONE', #19828, 10.99999999999999645 ) ;
#22159 = CARTESIAN_POINT ( 'NONE',  ( 39.00000000000000000, -29.49999999999999645, 11.00000000000000000 ) ) ;
#22160 = CARTESIAN_POINT ( 'NONE',  ( 40.49999999999998579, 50.99999999999999289, 12.50000000000000000 ) ) ;
#22161 = DIRECTION ( 'NONE',  ( 1.000000000000000000, 0.000000000000000000, 0.000000000000000000 ) ) ;
#22162 = LINE ( 'NONE', #14443, #17776 ) ;
#22163 = CARTESIAN_POINT ( 'NONE',  ( 7.022953521754877748, 5.102474405760673903, 8.833165578109190008 ) ) ;
#22164 = EDGE_CURVE ( 'NONE', #1531, #15821, #2203, .T. ) ;
#22165 = ORIENTED_EDGE ( 'NONE', *, *, #23862, .F. ) ;
#22166 = AXIS2_PLACEMENT_3D ( 'NONE', #22052, #8737, #8606 ) ;
#22167 = APPLICATION_PROTOCOL_DEFINITION ( 'draft international standard', 'automotive_design', 1998, #14437 ) ;
#22168 = CARTESIAN_POINT ( 'NONE',  ( -31.74999999999995737, 0.000000000000000000, 0.000000000000000000 ) ) ;
#22169 = VERTEX_POINT ( 'NONE', #9825 ) ;
#22170 = EDGE_LOOP ( 'NONE', ( #5678, #22251, #13140, #3397 ) ) ;
#22171 = ADVANCED_FACE ( 'NONE', ( #17529 ), #8240, .T. ) ;
#22172 = DIRECTION ( 'NONE',  ( 0.000000000000000000, -0.000000000000000000, -1.000000000000000000 ) ) ;
#22173 = CARTESIAN_POINT ( 'NONE',  ( -7.685661446561619314, -5.583959896779019161, -3.259589141758143516 ) ) ;
#22174 = EDGE_CURVE ( 'NONE', #8062, #17642, #1057, .T. ) ;
#22175 =( BOUNDED_CURVE ( )  B_SPLINE_CURVE ( 3, ( #1129, #8433, #21851, #19681 ),
 .UNSPECIFIED., .F., .T. ) 
 B_SPLINE_CURVE_WITH_KNOTS ( ( 4, 4 ),
 ( 0.000000000000000000, 1.570796326794897224 ),
 .UNSPECIFIED. ) 
 CURVE ( )  GEOMETRIC_REPRESENTATION_ITEM ( )  RATIONAL_B_SPLINE_CURVE ( ( 1.000000000000000000, 0.8047378541243649375, 0.8047378541243649375, 1.000000000000000000 ) ) 
 REPRESENTATION_ITEM ( '' )  );
#22176 = ORIENTED_EDGE ( 'NONE', *, *, #13087, .F. ) ;
#22177 = DIRECTION ( 'NONE',  ( -0.000000000000000000, -0.000000000000000000, -1.000000000000000000 ) ) ;
#22178 = DIRECTION ( 'NONE',  ( 1.000000000000000000, 0.000000000000000000, 0.000000000000000000 ) ) ;
#22179 = CARTESIAN_POINT ( 'NONE',  ( 41.00000000000000000, -4.000000000000015099, 9.500000000000000000 ) ) ;
#22180 = DIRECTION ( 'NONE',  ( -0.000000000000000000, -0.000000000000000000, -1.000000000000000000 ) ) ;
#22181 = DIRECTION ( 'NONE',  ( 1.000000000000000000, 0.000000000000000000, 0.000000000000000000 ) ) ;
#22182 = ORIENTED_EDGE ( 'NONE', *, *, #8278, .T. ) ;
#22183 = CARTESIAN_POINT ( 'NONE',  ( -2.935661446561384391, -9.035036904804158553, -6.606742014460233570 ) ) ;
#22184 = CIRCLE ( 'NONE', #21396, 1.500000000000001332 ) ;
#22185 = EDGE_LOOP ( 'NONE', ( #8238, #20868, #4232, #20795, #8188 ) ) ;
#22186 = CARTESIAN_POINT ( 'NONE',  ( 35.99999999999999289, -51.00000000000000711, 0.000000000000000000 ) ) ;
#22187 = DIRECTION ( 'NONE',  ( 0.000000000000000000, 0.000000000000000000, 1.000000000000000000 ) ) ;
#22188 = CARTESIAN_POINT ( 'NONE',  ( 0.000000000000000000, 45.00000000000000000, -3.000000000000000000 ) ) ;
#22189 = CARTESIAN_POINT ( 'NONE',  ( 16.81886298599062002, 7.518780870797758809, 5.825851398835383499 ) ) ;
#22190 = FACE_OUTER_BOUND ( 'NONE', #6567, .T. ) ;
#22191 = LINE ( 'NONE', #8761, #4404 ) ;
#22192 = CARTESIAN_POINT ( 'NONE',  ( -41.50000000000000000, -28.80990663662250739, 12.00000000000000000 ) ) ;
#22193 = ORIENTED_EDGE ( 'NONE', *, *, #7085, .F. ) ;
#22194 = ADVANCED_FACE ( 'NONE', ( #11780 ), #16230, .T. ) ;
#22195 = VERTEX_POINT ( 'NONE', #4368 ) ;
#22196 = CARTESIAN_POINT ( 'NONE',  ( 7.685661446561619314, 5.583959896779020049, 9.406742014460235168 ) ) ;
#22197 = ORIENTED_EDGE ( 'NONE', *, *, #11534, .F. ) ;
#22198 = ORIENTED_EDGE ( 'NONE', *, *, #23780, .F. ) ;
#22199 = ADVANCED_FACE ( 'NONE', ( #21334 ), #23606, .F. ) ;
#22200 = CARTESIAN_POINT ( 'NONE',  ( 23.00000000000000000, -11.55437235128774809, 1.752358929577604085 ) ) ;
#22201 = CARTESIAN_POINT ( 'NONE',  ( 28.99999999999999645, 29.49999999999999645, -3.000000000000000000 ) ) ;
#22202 = ADVANCED_FACE ( 'NONE', ( #10043 ), #7637, .T. ) ;
#22203 = VECTOR ( 'NONE', #11760, 1000.000000000000000 ) ;
#22204 = CYLINDRICAL_SURFACE ( 'NONE', #19642, 6.050000000006051870 ) ;
#22205 = SURFACE_SIDE_STYLE ('',( #17050 ) ) ;
#22206 = DIRECTION ( 'NONE',  ( -1.000000000000000000, -0.000000000000000000, 0.000000000000000000 ) ) ;
#22207 = CARTESIAN_POINT ( 'NONE',  ( 5.871322893123448239, 8.081182679344781405, -10.35958914175814449 ) ) ;
#22208 = ORIENTED_EDGE ( 'NONE', *, *, #18125, .F. ) ;
#22209 = CARTESIAN_POINT ( 'NONE',  ( 30.68762588338048403, 45.64284848299539732, -3.000000000000000000 ) ) ;
#22210 = DIRECTION ( 'NONE',  ( -0.000000000000000000, -0.000000000000000000, -1.000000000000000000 ) ) ;
#22211 = DIRECTION ( 'NONE',  ( 1.224646799147353207E-16, 1.000000000000000000, -0.000000000000000000 ) ) ;
#22212 = DIRECTION ( 'NONE',  ( -1.000000000000000000, -1.224606353822377258E-16, -0.000000000000000000 ) ) ;
#22213 = FACE_OUTER_BOUND ( 'NONE', #2655, .T. ) ;
#22214 = EDGE_CURVE ( 'NONE', #3150, #12663, #21690, .T. ) ;
#22215 = VECTOR ( 'NONE', #3131, 1000.000000000000000 ) ;
#22216 = DIRECTION ( 'NONE',  ( -0.000000000000000000, -0.000000000000000000, -1.000000000000000000 ) ) ;
#22217 = ORIENTED_EDGE ( 'NONE', *, *, #12616, .T. ) ;
#22218 = CARTESIAN_POINT ( 'NONE',  ( 60.03431729618309021, 7.562528597612068045E-15, 0.000000000000000000 ) ) ;
#22219 = ORIENTED_EDGE ( 'NONE', *, *, #6037, .T. ) ;
#22220 = CIRCLE ( 'NONE', #12462, 6.050000000006052758 ) ;
#22221 = EDGE_CURVE ( 'NONE', #16244, #8542, #13491, .T. ) ;
#22222 = FACE_OUTER_BOUND ( 'NONE', #22606, .T. ) ;
#22223 = CARTESIAN_POINT ( 'NONE',  ( 29.00000000000000355, -29.50000000000000000, -3.000000000000000000 ) ) ;
#22224 = ORIENTED_EDGE ( 'NONE', *, *, #13051, .F. ) ;
#22225 = FACE_OUTER_BOUND ( 'NONE', #22682, .T. ) ;
#22226 = CARTESIAN_POINT ( 'NONE',  ( 0.000000000000000000, 45.00000000000000000, 27.00000000000000000 ) ) ;
#22227 = EDGE_CURVE ( 'NONE', #16565, #1485, #15799, .T. ) ;
#22228 = CARTESIAN_POINT ( 'NONE',  ( 23.00000000000000000, 2.967071445749909220, 17.62702788437275458 ) ) ;
#22229 = EDGE_CURVE ( 'NONE', #23202, #19080, #19359, .T. ) ;
#22230 = CARTESIAN_POINT ( 'NONE',  ( 2.935661446561383503, 9.035036904804158553, -4.459589141758144137 ) ) ;
#22231 = ORIENTED_EDGE ( 'NONE', *, *, #4579, .T. ) ;
#22232 = ORIENTED_EDGE ( 'NONE', *, *, #13314, .T. ) ;
#22233 = CARTESIAN_POINT ( 'NONE',  ( -9.999999999999998224, 15.50000000000000178, 7.699999999999998401 ) ) ;
#22234 = AXIS2_PLACEMENT_3D ( 'NONE', #18943, #18460, #9284 ) ;
#22235 = ORIENTED_EDGE ( 'NONE', *, *, #2447, .T. ) ;
#22236 = CARTESIAN_POINT ( 'NONE',  ( -41.50000000000000000, 28.80990663662250739, 12.00000000000000000 ) ) ;
#22237 = ORIENTED_EDGE ( 'NONE', *, *, #13263, .F. ) ;
#22238 = CARTESIAN_POINT ( 'NONE',  ( 23.00000000000000000, -13.66196005206961850, -3.918670437617226110 ) ) ;
#22239 = CARTESIAN_POINT ( 'NONE',  ( -28.99999999999999645, -29.50000000000000000, -2.224999999999995204 ) ) ;
#22240 = DIRECTION ( 'NONE',  ( 0.000000000000000000, -0.000000000000000000, -1.000000000000000000 ) ) ;
#22241 = EDGE_LOOP ( 'NONE', ( #7003, #4463, #4464, #13938 ) ) ;
#22242 = DIRECTION ( 'NONE',  ( -6.485355633664482599E-14, 1.000000000000000000, 0.000000000000000000 ) ) ;
#22243 = EDGE_CURVE ( 'NONE', #3705, #7597, #17391, .T. ) ;
#22244 = CARTESIAN_POINT ( 'NONE',  ( 7.564539288232146497, -4.357045548396729195, 12.46583266205520246 ) ) ;
#22245 = CARTESIAN_POINT ( 'NONE',  ( 37.00000000000000711, 29.50000000000000355, 11.50000000000000000 ) ) ;
#22246 = EDGE_CURVE ( 'NONE', #5686, #12890, #15288, .T. ) ;
#22247 = CARTESIAN_POINT ( 'NONE',  ( -1.374911245008260563, 8.680847955710920161, 3.184419859656034024 ) ) ;
#22248 =( GEOMETRIC_REPRESENTATION_CONTEXT ( 3 ) GLOBAL_UNCERTAINTY_ASSIGNED_CONTEXT ( ( #11549 ) ) GLOBAL_UNIT_ASSIGNED_CONTEXT ( ( #5941, #14956, #3988 ) ) REPRESENTATION_CONTEXT ( 'NONE', 'WORKASPACE' ) );
#22249 = VERTEX_POINT ( 'NONE', #14198 ) ;
#22250 = ORIENTED_EDGE ( 'NONE', *, *, #3479, .F. ) ;
#22251 = ORIENTED_EDGE ( 'NONE', *, *, #22302, .F. ) ;
#22252 = LINE ( 'NONE', #20189, #5274 ) ;
#22253 = DIRECTION ( 'NONE',  ( -1.000000000000000000, 0.000000000000000000, 0.000000000000000000 ) ) ;
#22254 = ORIENTED_EDGE ( 'NONE', *, *, #6766, .F. ) ;
#22255 = FACE_OUTER_BOUND ( 'NONE', #14280, .T. ) ;
#22256 = LINE ( 'NONE', #14911, #15504 ) ;
#22257 = ORIENTED_EDGE ( 'NONE', *, *, #5132, .F. ) ;
#22258 = LINE ( 'NONE', #1881, #10826 ) ;
#22259 = AXIS2_PLACEMENT_3D ( 'NONE', #1708, #12432, #23914 ) ;
#22260 =( REPRESENTATION_RELATIONSHIP ('NONE','NONE', #21748, #2851 ) REPRESENTATION_RELATIONSHIP_WITH_TRANSFORMATION ( #403 )SHAPE_REPRESENTATION_RELATIONSHIP( ) );
#22261 = CARTESIAN_POINT ( 'NONE',  ( 68.76159002345582394, 7.562528597612068045E-15, 0.000000000000000000 ) ) ;
#22262 = AXIS2_PLACEMENT_3D ( 'NONE', #6291, #5930, #13736 ) ;
#22263 = LINE ( 'NONE', #16396, #11096 ) ;
#22264 = CARTESIAN_POINT ( 'NONE',  ( 5.078177448618334644, 1.377380391735521048E-15, -11.24716442891539714 ) ) ;
#22265 = LINE ( 'NONE', #9307, #7574 ) ;
#22266 = EDGE_CURVE ( 'NONE', #15606, #17955, #23834, .T. ) ;
#22267 = DIRECTION ( 'NONE',  ( 0.000000000000000000, -1.000000000000000000, 0.000000000000000000 ) ) ;
#22268 = EDGE_CURVE ( 'NONE', #19122, #2565, #2985, .T. ) ;
#22269 = CARTESIAN_POINT ( 'NONE',  ( -31.74999999999995737, 0.000000000000000000, 0.000000000000000000 ) ) ;
#22270 = ORIENTED_EDGE ( 'NONE', *, *, #9904, .F. ) ;
#22271 = EDGE_LOOP ( 'NONE', ( #5945, #12643, #5143, #23423, #17957 ) ) ;
#22272 = CARTESIAN_POINT ( 'NONE',  ( 8.680847955711007202, 5.912916378492122225E-13, 12.63316557810918894 ) ) ;
#22273 = EDGE_LOOP ( 'NONE', ( #6937, #8397, #10269, #17587 ) ) ;
#22274 = SHAPE_DEFINITION_REPRESENTATION ( #6918, #15290 ) ;
#22275 = AXIS2_PLACEMENT_3D ( 'NONE', #6693, #13643, #19764 ) ;
#22276 = ORIENTED_EDGE ( 'NONE', *, *, #15266, .F. ) ;
#22277 = ORIENTED_EDGE ( 'NONE', *, *, #15961, .F. ) ;
#22278 = AXIS2_PLACEMENT_3D ( 'NONE', #16360, #23819, #1613 ) ;
#22279 = DIRECTION ( 'NONE',  ( 1.000000000000000000, 0.000000000000000000, 0.000000000000000000 ) ) ;
#22280 = CARTESIAN_POINT ( 'NONE',  ( 8.680847955711007202, 5.912916378492122225E-13, -12.63316557810918894 ) ) ;
#22281 = AXIS2_PLACEMENT_3D ( 'NONE', #5318, #20559, #3361 ) ;
#22282 = ORIENTED_EDGE ( 'NONE', *, *, #5386, .T. ) ;
#22283 = FACE_OUTER_BOUND ( 'NONE', #2392, .T. ) ;
#22284 = CARTESIAN_POINT ( 'NONE',  ( 29.00000000000000355, -29.50000000000000000, -3.000000000000000000 ) ) ;
#22285 = LINE ( 'NONE', #12871, #19420 ) ;
#22286 = CARTESIAN_POINT ( 'NONE',  ( -34.00000000000000000, -3.999999999999999112, 10.49999999999999822 ) ) ;
#22287 = DIRECTION ( 'NONE',  ( 0.000000000000000000, 0.000000000000000000, 1.000000000000000000 ) ) ;
#22288 = ORIENTED_EDGE ( 'NONE', *, *, #872, .F. ) ;
#22289 = FACE_OUTER_BOUND ( 'NONE', #19360, .T. ) ;
#22290 = ADVANCED_FACE ( 'NONE', ( #3106 ), #1280, .T. ) ;
#22291 = ORIENTED_EDGE ( 'NONE', *, *, #15760, .F. ) ;
#22292 = EDGE_LOOP ( 'NONE', ( #20388, #12221, #16277, #15917 ) ) ;
#22293 = DIRECTION ( 'NONE',  ( -1.000000000000000000, -0.000000000000000000, -0.000000000000000000 ) ) ;
#22294 = DIRECTION ( 'NONE',  ( -1.000000000000000000, -0.000000000000000000, 0.000000000000000000 ) ) ;
#22295 = CYLINDRICAL_SURFACE ( 'NONE', #7841, 1.999999999999996669 ) ;
#22296 = CARTESIAN_POINT ( 'NONE',  ( 15.57833309066360350, 5.219313726039665369, 7.987432870209364211 ) ) ;
#22297 = ADVANCED_FACE ( 'NONE', ( #19589 ), #7116, .T. ) ;
#22298 = AXIS2_PLACEMENT_3D ( 'NONE', #1230, #4904, #6842 ) ;
#22299 = CARTESIAN_POINT ( 'NONE',  ( -30.32370777929697425, -42.16181938034195298, 0.000000000000000000 ) ) ;
#22300 = ADVANCED_FACE ( 'NONE', ( #8475 ), #21307, .F. ) ;
#22301 = CARTESIAN_POINT ( 'NONE',  ( 58.87477361290780919, -4.999999999999999112, 0.000000000000000000 ) ) ;
#22302 = EDGE_CURVE ( 'NONE', #19325, #18986, #22023, .T. ) ;
#22303 = EDGE_CURVE ( 'NONE', #7495, #17534, #3218, .T. ) ;
#22304 = CIRCLE ( 'NONE', #8258, 11.68650000001168898 ) ;
#22305 = VECTOR ( 'NONE', #8190, 1000.000000000000000 ) ;
#22306 = CYLINDRICAL_SURFACE ( 'NONE', #9755, 11.68650000001168721 ) ;
#22307 = ORIENTED_EDGE ( 'NONE', *, *, #9580, .T. ) ;
#22308 = ORIENTED_EDGE ( 'NONE', *, *, #21676, .T. ) ;
#22309 = CARTESIAN_POINT ( 'NONE',  ( 9.500000000000000000, 6.470877716354879437E-13, 11.20674201446023410 ) ) ;
#22310 = ORIENTED_EDGE ( 'NONE', *, *, #19217, .T. ) ;
#22311 = VERTEX_POINT ( 'NONE', #2998 ) ;
#22312 =( NAMED_UNIT ( * ) SI_UNIT ( $, .STERADIAN. ) SOLID_ANGLE_UNIT ( ) );
#22313 = ORIENTED_EDGE ( 'NONE', *, *, #6876, .F. ) ;
#22314 = DIRECTION ( 'NONE',  ( 0.000000000000000000, 0.000000000000000000, 1.000000000000000000 ) ) ;
#22315 = CYLINDRICAL_SURFACE ( 'NONE', #15408, 11.00000000000000355 ) ;
#22316 = DIRECTION ( 'NONE',  ( -0.000000000000000000, -0.000000000000000000, -1.000000000000000000 ) ) ;
#22317 = AXIS2_PLACEMENT_3D ( 'NONE', #15952, #14010, #3038 ) ;
#22318 = DIRECTION ( 'NONE',  ( 1.000000000000000000, 0.000000000000000000, 0.000000000000000000 ) ) ;
#22319 = AXIS2_PLACEMENT_3D ( 'NONE', #7207, #14650, #12811 ) ;
#22320 = AXIS2_PLACEMENT_3D ( 'NONE', #19766, #15958, #6817 ) ;
#22321 = AXIS2_PLACEMENT_3D ( 'NONE', #10482, #17691, #6599 ) ;
#22322 = VECTOR ( 'NONE', #5227, 1000.000000000000000 ) ;
#22323 = EDGE_CURVE ( 'NONE', #16134, #17802, #6507, .T. ) ;
#22324 = AXIS2_PLACEMENT_3D ( 'NONE', #12239, #21771, #1159 ) ;
#22325 = DIRECTION ( 'NONE',  ( 1.000000000000000000, 0.000000000000000000, 0.000000000000000000 ) ) ;
#22326 = CARTESIAN_POINT ( 'NONE',  ( -44.00000000000000711, -51.00000000000000711, 0.000000000000000000 ) ) ;
#22327 = DIRECTION ( 'NONE',  ( -1.000000000000000000, -1.224606353822377258E-16, -0.000000000000000000 ) ) ;
#22328 = AXIS2_PLACEMENT_3D ( 'NONE', #13227, #20815, #4335 ) ;
#22329 = CARTESIAN_POINT ( 'NONE',  ( -17.52854577772373190, 9.313395544511452684, -1.935253206038901608 ) ) ;
#22330 = CARTESIAN_POINT ( 'NONE',  ( 7.342598717236928252, 0.000000000000000000, 0.000000000000000000 ) ) ;
#22331 = LINE ( 'NONE', #16455, #6230 ) ;
#22332 = ADVANCED_FACE ( 'NONE', ( #23381 ), #4838, .T. ) ;
#22333 = CARTESIAN_POINT ( 'NONE',  ( -8.680847955710813579, -2.820578480814258437, -9.733165578109186811 ) ) ;
#22334 = EDGE_CURVE ( 'NONE', #8265, #16259, #22858, .T. ) ;
#22335 = DIRECTION ( 'NONE',  ( -1.000000000000000000, 0.000000000000000000, 0.000000000000000000 ) ) ;
#22336 = ORIENTED_EDGE ( 'NONE', *, *, #8016, .F. ) ;
#22337 = DIRECTION ( 'NONE',  ( 0.000000000000000000, 0.000000000000000000, 1.000000000000000000 ) ) ;
#22338 = ORIENTED_EDGE ( 'NONE', *, *, #23040, .F. ) ;
#22339 = CIRCLE ( 'NONE', #11783, 5.999999999999998224 ) ;
#22340 = CARTESIAN_POINT ( 'NONE',  ( 60.32931906745326245, 6.123233995736675563E-16, -5.000000000000007994 ) ) ;
#22341 = AXIS2_PLACEMENT_3D ( 'NONE', #4414, #13929, #8291 ) ;
#22342 = VECTOR ( 'NONE', #8835, 1000.000000000000000 ) ;
#22343 = ORIENTED_EDGE ( 'NONE', *, *, #4785, .F. ) ;
#22344 = DIRECTION ( 'NONE',  ( 0.000000000000000000, 0.000000000000000000, 1.000000000000000000 ) ) ;
#22345 = CONICAL_SURFACE ( 'NONE', #13374, 5.000000000000007994, 0.9599310885968855844 ) ;
#22346 = DIRECTION ( 'NONE',  ( -1.000000000000000000, -1.224606353822377258E-16, -0.000000000000000000 ) ) ;
#22347 = FACE_OUTER_BOUND ( 'NONE', #1222, .T. ) ;
#22348 = VECTOR ( 'NONE', #22843, 1000.000000000000000 ) ;
#22349 = CARTESIAN_POINT ( 'NONE',  ( 2.570122167802765922, 1.374779123446053458E-15, -11.22592346138681130 ) ) ;
#22350 = PLANE ( 'NONE',  #16478 ) ;
#22351 = CARTESIAN_POINT ( 'NONE',  ( 9.499999999999790390, 3.086737114213260025, -8.159589141758143427 ) ) ;
#22352 = ORIENTED_EDGE ( 'NONE', *, *, #2073, .F. ) ;
#22353 = ORIENTED_EDGE ( 'NONE', *, *, #13954, .F. ) ;
#22354 = FACE_OUTER_BOUND ( 'NONE', #12256, .T. ) ;
#22355 = ORIENTED_EDGE ( 'NONE', *, *, #21425, .T. ) ;
#22356 = CIRCLE ( 'NONE', #2081, 8.999999999999994671 ) ;
#22357 = DIRECTION ( 'NONE',  ( 0.000000000000000000, -1.000000000000000000, 0.000000000000000000 ) ) ;
#22358 = VECTOR ( 'NONE', #22993, 1000.000000000000000 ) ;
#22359 = CIRCLE ( 'NONE', #20395, 5.000000000000007994 ) ;
#22360 = VECTOR ( 'NONE', #8819, 1000.000000000000000 ) ;
#22361 = VECTOR ( 'NONE', #22042, 1000.000000000000000 ) ;
#22362 = ORIENTED_EDGE ( 'NONE', *, *, #23581, .F. ) ;
#22363 = EDGE_CURVE ( 'NONE', #12663, #22940, #4945, .T. ) ;
#22364 = CIRCLE ( 'NONE', #2481, 4.172000000000008590 ) ;
#22365 = DIRECTION ( 'NONE',  ( -1.000000000000000000, -0.000000000000000000, -0.000000000000000000 ) ) ;
#22366 = DIRECTION ( 'NONE',  ( -1.000000000000000000, -0.000000000000000000, -0.000000000000000000 ) ) ;
#22367 = CARTESIAN_POINT ( 'NONE',  ( 2.570122167802765922, 0.000000000000000000, 0.000000000000000000 ) ) ;
#22368 = EDGE_LOOP ( 'NONE', ( #20774, #12198 ) ) ;
#22369 = CARTESIAN_POINT ( 'NONE',  ( 0.000000000000000000, 15.50000000000000000, 7.700000000000001954 ) ) ;
#22370 = CARTESIAN_POINT ( 'NONE',  ( 33.99999999999998579, 4.999999999999985789, 11.00000000000000000 ) ) ;
#22371 = CARTESIAN_POINT ( 'NONE',  ( 63.23840997654417606, -4.999999999999989342, 0.000000000000000000 ) ) ;
#22372 = DIRECTION ( 'NONE',  ( -1.000000000000000000, 2.600433232233976523E-16, 0.000000000000000000 ) ) ;
#22373 = DIRECTION ( 'NONE',  ( -0.000000000000000000, -1.000000000000000000, -0.000000000000000000 ) ) ;
#22374 = ORIENTED_EDGE ( 'NONE', *, *, #12940, .F. ) ;
#22375 = ORIENTED_EDGE ( 'NONE', *, *, #14565, .F. ) ;
#22376 = VECTOR ( 'NONE', #284, 1000.000000000000000 ) ;
#22377 = ORIENTED_EDGE ( 'NONE', *, *, #19789, .T. ) ;
#22378 = VECTOR ( 'NONE', #20875, 1000.000000000000000 ) ;
#22380 = ORIENTED_EDGE ( 'NONE', *, *, #19540, .F. ) ;
#22379 = AXIS2_PLACEMENT_3D ( 'NONE', #13840, #21288, #11730 ) ;
#22381 = DIRECTION ( 'NONE',  ( 1.000000000000000000, 0.000000000000000000, 0.000000000000000000 ) ) ;
#22382 = EDGE_CURVE ( 'NONE', #19429, #15518, #1170, .T. ) ;
#22383 = AXIS2_PLACEMENT_3D ( 'NONE', #5049, #12820, #12461 ) ;
#22384 = CARTESIAN_POINT ( 'NONE',  ( 23.00000000000000000, -9.374578970469563899, -10.68280860024325030 ) ) ;
#22385 = ORIENTED_EDGE ( 'NONE', *, *, #2665, .T. ) ;
#22386 = EDGE_CURVE ( 'NONE', #10579, #5147, #19939, .T. ) ;
#22387 = DIRECTION ( 'NONE',  ( -1.000000000000000000, 0.000000000000000000, 0.000000000000000000 ) ) ;
#22388 = ORIENTED_EDGE ( 'NONE', *, *, #5531, .F. ) ;
#22389 = CARTESIAN_POINT ( 'NONE',  ( -40.23082370883258108, -27.62204025492846071, -3.000000000000000000 ) ) ;
#22390 = EDGE_CURVE ( 'NONE', #5827, #13474, #12369, .T. ) ;
#22391 = DIRECTION ( 'NONE',  ( -1.000000000000000000, -0.000000000000000000, -0.000000000000000000 ) ) ;
#22392 = CARTESIAN_POINT ( 'NONE',  ( 0.000000000000000000, 0.000000000000000000, 6.500000000000000888 ) ) ;
#22393 = CARTESIAN_POINT ( 'NONE',  ( -41.00000000000000000, 6.000000000000000888, 11.00000000000000000 ) ) ;
#22394 = CIRCLE ( 'NONE', #11069, 1.000000000000000888 ) ;
#22395 = CARTESIAN_POINT ( 'NONE',  ( 30.32370777929699202, 42.16181938034194587, -1.500000000000000000 ) ) ;
#22396 = ORIENTED_EDGE ( 'NONE', *, *, #21912, .T. ) ;
#22397 = ORIENTED_EDGE ( 'NONE', *, *, #1949, .T. ) ;
#22398 = DIRECTION ( 'NONE',  ( -1.000000000000000000, -1.224606353822377258E-16, -0.000000000000000000 ) ) ;
#22399 = DIRECTION ( 'NONE',  ( 1.000000000000000000, 0.000000000000000000, 0.000000000000000000 ) ) ;
#22400 = CARTESIAN_POINT ( 'NONE',  ( 60.90909090909091361, -4.172000000000000597, 5.616230220889771312E-16 ) ) ;
#22401 = ORIENTED_EDGE ( 'NONE', *, *, #8038, .F. ) ;
#22402 = VECTOR ( 'NONE', #18877, 1000.000000000000000 ) ;
#22403 = CARTESIAN_POINT ( 'NONE',  ( 5.365059087798938364, 7.384370330707087149, 4.933165578109187877 ) ) ;
#22404 = ORIENTED_EDGE ( 'NONE', *, *, #3669, .F. ) ;
#22405 = APPLICATION_PROTOCOL_DEFINITION ( 'draft international standard', 'automotive_design', 1998, #12741 ) ;
#22406 = VECTOR ( 'NONE', #8962, 1000.000000000000114 ) ;
#22407 = EDGE_LOOP ( 'NONE', ( #5838, #4332, #7816, #91 ) ) ;
#22408 = VERTEX_POINT ( 'NONE', #8579 ) ;
#22409 = CARTESIAN_POINT ( 'NONE',  ( 33.99999999999998579, -1.387778780781445676E-14, 12.00000000000000000 ) ) ;
#22410 = CARTESIAN_POINT ( 'NONE',  ( -2.935661446562617183, 9.035036904803758873, -2.659589141758143871 ) ) ;
#22411 = CARTESIAN_POINT ( 'NONE',  ( 33.99999999999998579, -5.000000000000013323, 10.49999999999999822 ) ) ;
#22412 = CIRCLE ( 'NONE', #11866, 1.499999999999998002 ) ;
#22413 = ORIENTED_EDGE ( 'NONE', *, *, #7159, .T. ) ;
#22414 = DIRECTION ( 'NONE',  ( 0.000000000000000000, -0.9898214418809342385, 0.1423148382732755957 ) ) ;
#22415 = DIRECTION ( 'NONE',  ( -1.000000000000000000, 0.000000000000000000, 0.000000000000000000 ) ) ;
#22416 = PLANE ( 'NONE',  #8887 ) ;
#22417 = EDGE_CURVE ( 'NONE', #18344, #13385, #20145, .T. ) ;
#22418 = EDGE_CURVE ( 'NONE', #20829, #13157, #8440, .T. ) ;
#22419 = CARTESIAN_POINT ( 'NONE',  ( 31.10231664966676846, -45.36128193761570770, 11.00000000000000000 ) ) ;
#22420 = AXIS2_PLACEMENT_3D ( 'NONE', #10176, #941, #19373 ) ;
#22421 = CARTESIAN_POINT ( 'NONE',  ( 79.23840997654417606, -4.999999999999989342, 0.000000000000000000 ) ) ;
#22422 = ORIENTED_EDGE ( 'NONE', *, *, #1929, .F. ) ;
#22423 = DIRECTION ( 'NONE',  ( 1.000000000000000000, 0.000000000000000000, 0.000000000000000000 ) ) ;
#22424 = VERTEX_POINT ( 'NONE', #23730 ) ;
#22425 = FACE_OUTER_BOUND ( 'NONE', #2251, .T. ) ;
#22426 = DIRECTION ( 'NONE',  ( 1.000000000000000000, 0.000000000000000000, 0.000000000000000000 ) ) ;
#22427 = CYLINDRICAL_SURFACE ( 'NONE', #17656, 6.050000000006051870 ) ;
#22428 = DIRECTION ( 'NONE',  ( -0.8757121056631642642, 0.4828336235133043886, -0.000000000000000000 ) ) ;
#22429 = CIRCLE ( 'NONE', #4516, 4.172000000000008590 ) ;
#22430 = ADVANCED_BREP_SHAPE_REPRESENTATION ( '', ( #2929, #8005 ), #13887 ) ;
#22431 = AXIS2_PLACEMENT_3D ( 'NONE', #15700, #15572, #6452 ) ;
#22432 = LINE ( 'NONE', #5715, #18891 ) ;
#22433 = CARTESIAN_POINT ( 'NONE',  ( 6.222797240145152671E-13, -9.127583699786111282, -12.13316557810918717 ) ) ;
#22434 = CARTESIAN_POINT ( 'NONE',  ( 7.685661446562381371, -5.583959896777971110, 9.006742014460233037 ) ) ;
#22435 = ORIENTED_EDGE ( 'NONE', *, *, #1443, .F. ) ;
#22436 = VERTEX_POINT ( 'NONE', #14426 ) ;
#22437 = ORIENTED_EDGE ( 'NONE', *, *, #1359, .F. ) ;
#22438 = PRODUCT_DEFINITION ( 'UNKNOWN', '', #2185, #2617 ) ;
#22439 = ORIENTED_EDGE ( 'NONE', *, *, #15585, .F. ) ;
#22440 = EDGE_CURVE ( 'NONE', #19859, #23418, #11542, .T. ) ;
#22441 = AXIS2_PLACEMENT_3D ( 'NONE', #15357, #490, #265 ) ;
#22442 = ORIENTED_EDGE ( 'NONE', *, *, #18212, .T. ) ;
#22443 = CARTESIAN_POINT ( 'NONE',  ( 86.21613547800127719, 7.562528597612068045E-15, 0.000000000000000000 ) ) ;
#22444 = CONICAL_SURFACE ( 'NONE', #2564, 1.999999999999994449, 1.029744258676653201 ) ;
#22445 = EDGE_CURVE ( 'NONE', #4924, #11720, #14668, .T. ) ;
#22446 = VECTOR ( 'NONE', #2857, 1000.000000000000000 ) ;
#22447 = DIRECTION ( 'NONE',  ( 0.000000000000000000, 0.000000000000000000, 1.000000000000000000 ) ) ;
#22448 = DIRECTION ( 'NONE',  ( -0.000000000000000000, -0.000000000000000000, -1.000000000000000000 ) ) ;
#22449 = EDGE_CURVE ( 'NONE', #3391, #23772, #7352, .T. ) ;
#22450 = EDGE_CURVE ( 'NONE', #12080, #13274, #18704, .T. ) ;
#22451 = ORIENTED_EDGE ( 'NONE', *, *, #149, .F. ) ;
#22452 = FACE_OUTER_BOUND ( 'NONE', #5773, .T. ) ;
#22453 = VECTOR ( 'NONE', #17049, 1000.000000000000000 ) ;
#22454 = CARTESIAN_POINT ( 'NONE',  ( -0.9830802669677229932, 45.00000000000000000, 3.000000000000002665 ) ) ;
#22455 = CARTESIAN_POINT ( 'NONE',  ( -17.57797814737054054, 9.461914562436916754, -0.9781177603712974955 ) ) ;
#22456 =( GEOMETRIC_REPRESENTATION_CONTEXT ( 3 ) GLOBAL_UNCERTAINTY_ASSIGNED_CONTEXT ( ( #23031 ) ) GLOBAL_UNIT_ASSIGNED_CONTEXT ( ( #5012, #12308, #16435 ) ) REPRESENTATION_CONTEXT ( 'NONE', 'WORKASPACE' ) );
#22457 = AXIS2_PLACEMENT_3D ( 'NONE', #13918, #21361, #4651 ) ;
#22458 = CARTESIAN_POINT ( 'NONE',  ( 42.00000000000000000, 25.22443390181681622, -1.500000000000000000 ) ) ;
#22459 = ORIENTED_EDGE ( 'NONE', *, *, #13899, .F. ) ;
#22460 = VECTOR ( 'NONE', #21835, 1000.000000000000000 ) ;
#22461 = FACE_OUTER_BOUND ( 'NONE', #1165, .T. ) ;
#22462 = AXIS2_PLACEMENT_3D ( 'NONE', #16331, #10718, #16098 ) ;
#22463 = VERTEX_POINT ( 'NONE', #1874 ) ;
#22464 = CYLINDRICAL_SURFACE ( 'NONE', #10683, 23.84999999999999432 ) ;
#22465 = ORIENTED_EDGE ( 'NONE', *, *, #17424, .T. ) ;
#22466 = CYLINDRICAL_SURFACE ( 'NONE', #8685, 5.000000000000000888 ) ;
#22467 = ORIENTED_EDGE ( 'NONE', *, *, #21850, .T. ) ;
#22468 = DIRECTION ( 'NONE',  ( -1.000000000000000000, -0.000000000000000000, -0.000000000000000000 ) ) ;
#22469 = EDGE_CURVE ( 'NONE', #13972, #19865, #9059, .T. ) ;
#22470 = DIRECTION ( 'NONE',  ( -1.000000000000000000, 0.000000000000000000, 0.000000000000000000 ) ) ;
#22471 = DIRECTION ( 'NONE',  ( -1.000000000000000000, 0.000000000000000000, 0.000000000000000000 ) ) ;
#22472 = AXIS2_PLACEMENT_3D ( 'NONE', #7382, #7737, #18626 ) ;
#22473 = AXIS2_PLACEMENT_3D ( 'NONE', #21664, #18236, #14556 ) ;
#22474 = CARTESIAN_POINT ( 'NONE',  ( -35.99999999999995026, 59.99999999999998579, 0.000000000000000000 ) ) ;
#22475 = EDGE_CURVE ( 'NONE', #8263, #3022, #13198, .T. ) ;
#22476 = EDGE_CURVE ( 'NONE', #13857, #2378, #15430, .T. ) ;
#22477 = CYLINDRICAL_SURFACE ( 'NONE', #15326, 9.725923461386811297 ) ;
#22478 = AXIS2_PLACEMENT_3D ( 'NONE', #6706, #8634, #17686 ) ;
#22479 = CARTESIAN_POINT ( 'NONE',  ( -9.500000000000000000, -6.482511860946779655E-13, -7.059589141758143782 ) ) ;
#22480 = ORIENTED_EDGE ( 'NONE', *, *, #8800, .T. ) ;
#22481 = DIRECTION ( 'NONE',  ( -0.000000000000000000, 0.000000000000000000, 1.000000000000000000 ) ) ;
#22482 = CARTESIAN_POINT ( 'NONE',  ( 0.000000000000000000, 0.000000000000000000, 2.500000000000000000 ) ) ;
#22483 = ORIENTED_EDGE ( 'NONE', *, *, #21733, .T. ) ;
#22484 = CARTESIAN_POINT ( 'NONE',  ( 2.935661446561383503, 9.035036904804158553, 5.606742014460233570 ) ) ;
#22485 = CARTESIAN_POINT ( 'NONE',  ( 6.999999999999999112, 1.717680227207312385E-15, -14.02592346138681201 ) ) ;
#22486 = CARTESIAN_POINT ( 'NONE',  ( 14.91530227160598798, 1.623290104782669330, -9.365835742197232250 ) ) ;
#22487 = CARTESIAN_POINT ( 'NONE',  ( -2.694088866357877254, 8.587672555557725573, 79.66581864099087795 ) ) ;
#22488 = AXIS2_PLACEMENT_3D ( 'NONE', #650, #15759, #22972 ) ;
#22489 = FACE_BOUND ( 'NONE', #15076, .T. ) ;
#22490 = DIRECTION ( 'NONE',  ( 0.000000000000000000, 0.000000000000000000, 1.000000000000000000 ) ) ;
#22491 = DIRECTION ( 'NONE',  ( -1.000000000000000000, 0.000000000000000000, 0.000000000000000000 ) ) ;
#22492 = VERTEX_POINT ( 'NONE', #10879 ) ;
#22493 = DIRECTION ( 'NONE',  ( -1.000000000000000000, 0.000000000000000000, 0.000000000000000000 ) ) ;
#22494 = CARTESIAN_POINT ( 'NONE',  ( 23.00000000000000000, -7.812991839788868909, 16.07708877602010489 ) ) ;
#22495 = DIRECTION ( 'NONE',  ( -1.000000000000000000, -1.224606353822377258E-16, -0.000000000000000000 ) ) ;
#22496 = FACE_OUTER_BOUND ( 'NONE', #7708, .T. ) ;
#22497 = ORIENTED_EDGE ( 'NONE', *, *, #1917, .F. ) ;
#22498 = CONTEXT_DEPENDENT_SHAPE_REPRESENTATION ( #11796, #10792 ) ;
#22499 = ORIENTED_EDGE ( 'NONE', *, *, #22586, .T. ) ;
#22500 = DIRECTION ( 'NONE',  ( 0.7071067811865469066, 0.000000000000000000, 0.7071067811865482389 ) ) ;
#22501 = EDGE_CURVE ( 'NONE', #23937, #6532, #22252, .T. ) ;
#22502 = EDGE_CURVE ( 'NONE', #17379, #13780, #13086, .T. ) ;
#22503 = CARTESIAN_POINT ( 'NONE',  ( 71.09090909090909349, 7.491529369508391930E-15, 0.000000000000000000 ) ) ;
#22504 = ORIENTED_EDGE ( 'NONE', *, *, #11949, .T. ) ;
#22505 = DIRECTION ( 'NONE',  ( 0.000000000000000000, -1.000000000000000000, 0.000000000000000000 ) ) ;
#22506 = CARTESIAN_POINT ( 'NONE',  ( 35.99999999999999289, 50.99999999999999289, 12.50000000000000000 ) ) ;
#22507 = ORIENTED_EDGE ( 'NONE', *, *, #17278, .F. ) ;
#22508 = CARTESIAN_POINT ( 'NONE',  ( 42.00000000000000000, -26.82133436441678853, 0.000000000000000000 ) ) ;
#22509 = LINE ( 'NONE', #13585, #15639 ) ;
#22510 = CARTESIAN_POINT ( 'NONE',  ( -34.02499999999999858, -29.50000000000000000, -3.000000000000000000 ) ) ;
#22511 = FACE_OUTER_BOUND ( 'NONE', #11138, .T. ) ;
#22512 = CARTESIAN_POINT ( 'NONE',  ( -30.31394790604173650, 39.41330121100982353, 11.00000000000000000 ) ) ;
#22513 = EDGE_LOOP ( 'NONE', ( #13136, #11976, #11571, #8388, #22557 ) ) ;
#22514 = ORIENTED_EDGE ( 'NONE', *, *, #19579, .F. ) ;
#22515 = DIRECTION ( 'NONE',  ( -1.000000000000000000, 0.000000000000000000, -0.000000000000000000 ) ) ;
#22516 = DIRECTION ( 'NONE',  ( -0.000000000000000000, -1.000000000000000000, -0.000000000000000000 ) ) ;
#22517 = ADVANCED_FACE ( 'NONE', ( #11231 ), #18908, .T. ) ;
#22518 = ORIENTED_EDGE ( 'NONE', *, *, #19759, .T. ) ;
#22519 = ORIENTED_EDGE ( 'NONE', *, *, #19331, .F. ) ;
#22520 = CARTESIAN_POINT ( 'NONE',  ( 7.022953521754877748, 5.102474405760673903, 6.833165578109188232 ) ) ;
#22521 = ORIENTED_EDGE ( 'NONE', *, *, #9987, .T. ) ;
#22522 = EDGE_CURVE ( 'NONE', #2924, #1880, #11478, .T. ) ;
#22523 = PRODUCT_CONTEXT ( 'NONE', #8195, 'mechanical' ) ;
#22524 = VERTEX_POINT ( 'NONE', #9186 ) ;
#22525 = ORIENTED_EDGE ( 'NONE', *, *, #15175, .F. ) ;
#22526 = ADVANCED_FACE ( 'NONE', ( #50 ), #18470, .F. ) ;
#22527 = DIRECTION ( 'NONE',  ( 1.000000000000000000, 1.224606353822377258E-16, 0.000000000000000000 ) ) ;
#22528 = CARTESIAN_POINT ( 'NONE',  ( -8.680847955711200825, 2.820578480813073607, -7.533165578109188409 ) ) ;
#22529 = EDGE_CURVE ( 'NONE', #10776, #11642, #24031, .T. ) ;
#22530 = ORIENTED_EDGE ( 'NONE', *, *, #17053, .T. ) ;
#22531 = CARTESIAN_POINT ( 'NONE',  ( 30.16774287754692807, 40.66994976491903913, -3.000000000000000000 ) ) ;
#22532 = DIRECTION ( 'NONE',  ( -0.000000000000000000, -0.000000000000000000, -1.000000000000000000 ) ) ;
#22533 = DIRECTION ( 'NONE',  ( 0.000000000000000000, 0.000000000000000000, -1.000000000000000000 ) ) ;
#22534 = DIRECTION ( 'NONE',  ( -1.000000000000000000, 0.000000000000000000, 0.000000000000000000 ) ) ;
#22535 = AXIS2_PLACEMENT_3D ( 'NONE', #9324, #3743, #16545 ) ;
#22536 = DIRECTION ( 'NONE',  ( -1.000000000000000000, -0.000000000000000000, 0.000000000000000000 ) ) ;
#22537 = EDGE_LOOP ( 'NONE', ( #18836, #17790 ) ) ;
#22538 = CARTESIAN_POINT ( 'NONE',  ( -9.500000000000000000, -6.482511860946779655E-13, -7.059589141758143782 ) ) ;
#22539 = ORIENTED_EDGE ( 'NONE', *, *, #18708, .F. ) ;
#22540 = DIRECTION ( 'NONE',  ( 0.000000000000000000, 0.000000000000000000, 1.000000000000000000 ) ) ;
#22541 = DIRECTION ( 'NONE',  ( -1.000000000000000000, -1.224606353822377258E-16, -0.000000000000000000 ) ) ;
#22542 = DIRECTION ( 'NONE',  ( 0.000000000000000000, -1.000000000000000000, 0.000000000000000000 ) ) ;
#22543 = CYLINDRICAL_SURFACE ( 'NONE', #11848, 1.000000000000002442 ) ;
#22544 = CARTESIAN_POINT ( 'NONE',  ( -7.022953521755574080, 5.102474405759713783, -11.43316557810918965 ) ) ;
#22545 = ORIENTED_EDGE ( 'NONE', *, *, #12393, .T. ) ;
#22546 = ORIENTED_EDGE ( 'NONE', *, *, #7133, .F. ) ;
#22547 = ADVANCED_FACE ( 'NONE', ( #1980, #14685 ), #22148, .T. ) ;
#22548 = ORIENTED_EDGE ( 'NONE', *, *, #3668, .T. ) ;
#22549 = ORIENTED_EDGE ( 'NONE', *, *, #15724, .F. ) ;
#22550 = DIRECTION ( 'NONE',  ( -0.000000000000000000, -0.000000000000000000, -1.000000000000000000 ) ) ;
#22551 = UNCERTAINTY_MEASURE_WITH_UNIT (LENGTH_MEASURE( 1.000000000000000082E-05 ), #5601, 'distance_accuracy_value', 'NONE');
#22552 = DIRECTION ( 'NONE',  ( -0.000000000000000000, -0.000000000000000000, -1.000000000000000000 ) ) ;
#22553 = LINE ( 'NONE', #9601, #4127 ) ;
#22554 = FACE_OUTER_BOUND ( 'NONE', #23687, .T. ) ;
#22555 = CARTESIAN_POINT ( 'NONE',  ( 9.999999999999998224, 1.224646799147353059E-15, 0.000000000000000000 ) ) ;
#22556 = DIRECTION ( 'NONE',  ( -0.000000000000000000, -1.000000000000000000, -0.000000000000000000 ) ) ;
#22557 = ORIENTED_EDGE ( 'NONE', *, *, #12887, .T. ) ;
#22558 = FACE_OUTER_BOUND ( 'NONE', #12764, .T. ) ;
#22559 = PLANE ( 'NONE',  #17593 ) ;
#22560 = DIRECTION ( 'NONE',  ( 0.000000000000000000, -1.000000000000000000, 0.000000000000000000 ) ) ;
#22561 = CARTESIAN_POINT ( 'NONE',  ( 68.76159002345582394, 6.123233995736675563E-16, -5.000000000000007994 ) ) ;
#22562 = ORIENTED_EDGE ( 'NONE', *, *, #4827, .F. ) ;
#22563 = EDGE_CURVE ( 'NONE', #21329, #13407, #23205, .T. ) ;
#22564 = ORIENTED_EDGE ( 'NONE', *, *, #22243, .T. ) ;
#22565 = CARTESIAN_POINT ( 'NONE',  ( 12.50000000000000178, 5.755434930044642846E-15, 2.500000000000000000 ) ) ;
#22566 = ORIENTED_EDGE ( 'NONE', *, *, #22891, .T. ) ;
#22567 = CARTESIAN_POINT ( 'NONE',  ( 5.871322893123449127, 8.081182679344781405, 10.35958914175814627 ) ) ;
#22568 = EDGE_CURVE ( 'NONE', #5790, #15957, #20415, .T. ) ;
#22569 = EDGE_CURVE ( 'NONE', #10096, #10996, #3003, .T. ) ;
#22570 = EDGE_LOOP ( 'NONE', ( #22920, #41, #17930, #318, #4285 ) ) ;
#22571 = DIRECTION ( 'NONE',  ( -0.000000000000000000, -0.000000000000000000, 1.000000000000000000 ) ) ;
#22572 = CARTESIAN_POINT ( 'NONE',  ( -6.153822176767817416E-13, 9.500000000000000000, -2.559589141758142894 ) ) ;
#22573 = DIRECTION ( 'NONE',  ( -0.000000000000000000, -0.000000000000000000, -1.000000000000000000 ) ) ;
#22574 = DIRECTION ( 'NONE',  ( -1.000000000000000000, -0.000000000000000000, -0.000000000000000000 ) ) ;
#22575 =( REPRESENTATION_RELATIONSHIP ('NONE','NONE', #12815, #17018 ) REPRESENTATION_RELATIONSHIP_WITH_TRANSFORMATION ( #6135 )SHAPE_REPRESENTATION_RELATIONSHIP( ) );
#22576 = CYLINDRICAL_SURFACE ( 'NONE', #20742, 1.999999999999994449 ) ;
#22577 = AXIS2_PLACEMENT_3D ( 'NONE', #10426, #2873, #13980 ) ;
#22578 = CARTESIAN_POINT ( 'NONE',  ( 5.871322893124553133, -8.081182679343980269, -5.759589141758144848 ) ) ;
#22579 = ORIENTED_EDGE ( 'NONE', *, *, #8113, .F. ) ;
#22580 = CARTESIAN_POINT ( 'NONE',  ( 0.000000000000000000, 0.000000000000000000, 3.699999999999998845 ) ) ;
#22581 = ORIENTED_EDGE ( 'NONE', *, *, #21804, .F. ) ;
#22582 = LINE ( 'NONE', #10661, #132 ) ;
#22583 = AXIS2_PLACEMENT_3D ( 'NONE', #4645, #15720, #614 ) ;
#22584 = CARTESIAN_POINT ( 'NONE',  ( 41.00000000000000000, 3.999999999999987121, 8.500000000000000000 ) ) ;
#22585 = DIRECTION ( 'NONE',  ( 0.000000000000000000, 0.000000000000000000, -1.000000000000000000 ) ) ;
#22586 = EDGE_CURVE ( 'NONE', #20973, #2336, #15788, .T. ) ;
#22587 = AXIS2_PLACEMENT_3D ( 'NONE', #19167, #15120, #17200 ) ;
#22588 = CARTESIAN_POINT ( 'NONE',  ( 11.50000000000000000, 11.37860023611358962, -13.78561139983841599 ) ) ;
#22589 = CARTESIAN_POINT ( 'NONE',  ( -0.1971285389010652422, 9.000000000000000000, 77.99999999999998579 ) ) ;
#22590 = DIRECTION ( 'NONE',  ( -1.000000000000000000, -0.000000000000000000, -0.000000000000000000 ) ) ;
#22591 = DIRECTION ( 'NONE',  ( 0.000000000000000000, 0.000000000000000000, 1.000000000000000000 ) ) ;
#22592 = ADVANCED_FACE ( 'NONE', ( #7579 ), #20297, .T. ) ;
#22593 = PLANE ( 'NONE',  #20011 ) ;
#22594 = ORIENTED_EDGE ( 'NONE', *, *, #16099, .T. ) ;
#22595 = DIRECTION ( 'NONE',  ( -1.000000000000000000, -1.224606353822377258E-16, -0.000000000000000000 ) ) ;
#22596 = DIRECTION ( 'NONE',  ( 0.7071067811865660024, 0.000000000000000000, 0.7071067811865291430 ) ) ;
#22597 = EDGE_CURVE ( 'NONE', #15649, #22724, #13452, .T. ) ;
#22598 = DIRECTION ( 'NONE',  ( -0.000000000000000000, -0.000000000000000000, -1.000000000000000000 ) ) ;
#22599 = ADVANCED_FACE ( 'NONE', ( #18957 ), #22816, .T. ) ;
#22600 = EDGE_CURVE ( 'NONE', #8001, #192, #23613, .T. ) ;
#22601 = FACE_OUTER_BOUND ( 'NONE', #3084, .T. ) ;
#22602 = DIRECTION ( 'NONE',  ( 1.000000000000000000, 0.000000000000000000, 0.000000000000000000 ) ) ;
#22603 = ORIENTED_EDGE ( 'NONE', *, *, #23637, .F. ) ;
#22604 = ORIENTED_EDGE ( 'NONE', *, *, #5463, .F. ) ;
#22606 = EDGE_LOOP ( 'NONE', ( #23240, #3452, #6311, #14731 ) ) ;
#22605 = CIRCLE ( 'NONE', #17143, 5.099999999999996980 ) ;
#22607 = EDGE_LOOP ( 'NONE', ( #12145, #22941 ) ) ;
#22608 = DIRECTION ( 'NONE',  ( -0.000000000000000000, 0.000000000000000000, -1.000000000000000000 ) ) ;
#22609 = CARTESIAN_POINT ( 'NONE',  ( -18.50000000000000000, 15.23000000000000220, 27.00000000000000000 ) ) ;
#22610 = ORIENTED_EDGE ( 'NONE', *, *, #346, .T. ) ;
#22611 = ORIENTED_EDGE ( 'NONE', *, *, #2218, .F. ) ;
#22612 = CARTESIAN_POINT ( 'NONE',  ( 0.000000000000000000, 0.000000000000000000, 103.9999999999999858 ) ) ;
#22613 = VERTEX_POINT ( 'NONE', #17473 ) ;
#22614 = EDGE_CURVE ( 'NONE', #16185, #13109, #523, .T. ) ;
#22615 = ORIENTED_EDGE ( 'NONE', *, *, #24038, .F. ) ;
#22616 = PLANE ( 'NONE',  #8234 ) ;
#22617 = DIRECTION ( 'NONE',  ( 0.5735764363510427177, -0.8191520442889941300, 1.003171929053527705E-16 ) ) ;
#22618 = CARTESIAN_POINT ( 'NONE',  ( 42.00000000000000000, -26.82133436441678853, 12.00000000000000000 ) ) ;
#22619 = LINE ( 'NONE', #16871, #1367 ) ;
#22620 = VECTOR ( 'NONE', #20471, 1000.000000000000000 ) ;
#22621 = ORIENTED_EDGE ( 'NONE', *, *, #13088, .T. ) ;
#22622 = DIRECTION ( 'NONE',  ( -1.000000000000000000, -0.000000000000000000, 0.000000000000000000 ) ) ;
#22623 = DIRECTION ( 'NONE',  ( 0.7052211081716915908, -0.7089874389501490404, 0.000000000000000000 ) ) ;
#22624 = CARTESIAN_POINT ( 'NONE',  ( 1.999999999999994449, 45.00000000000000000, -23.99999999999999645 ) ) ;
#22625 = ORIENTED_EDGE ( 'NONE', *, *, #762, .T. ) ;
#22626 = ADVANCED_FACE ( 'NONE', ( #5885 ), #22977, .F. ) ;
#22627 = ORIENTED_EDGE ( 'NONE', *, *, #7082, .F. ) ;
#22628 = CARTESIAN_POINT ( 'NONE',  ( 8.680847955710813579, 2.820578480814259326, 4.733165578109188587 ) ) ;
#22629 = ORIENTED_EDGE ( 'NONE', *, *, #16755, .T. ) ;
#22630 = CARTESIAN_POINT ( 'NONE',  ( 9.500000000000000000, 6.470877716354879437E-13, 6.059589141758143782 ) ) ;
#22631 = VERTEX_POINT ( 'NONE', #22866 ) ;
#22632 = ORIENTED_EDGE ( 'NONE', *, *, #2766, .F. ) ;
#22633 = DIRECTION ( 'NONE',  ( -1.000000000000000000, -1.224606353822377258E-16, -0.000000000000000000 ) ) ;
#22634 = CARTESIAN_POINT ( 'NONE',  ( 2.682529543899157876, 8.255977015246598327, -11.03316557810918752 ) ) ;
#22635 = DIRECTION ( 'NONE',  ( -0.8571673007021121116, 0.000000000000000000, -0.5150380749100544886 ) ) ;
#22636 = CIRCLE ( 'NONE', #4321, 4.057500000000000107 ) ;
#22637 = ORIENTED_EDGE ( 'NONE', *, *, #18278, .F. ) ;
#22638 = DIRECTION ( 'NONE',  ( -1.000000000000000000, -0.000000000000000000, -0.000000000000000000 ) ) ;
#22639 = FACE_OUTER_BOUND ( 'NONE', #7897, .T. ) ;
#22640 = FACE_OUTER_BOUND ( 'NONE', #4187, .T. ) ;
#22641 = FACE_OUTER_BOUND ( 'NONE', #10419, .T. ) ;
#22642 = AXIS2_PLACEMENT_3D ( 'NONE', #10206, #17669, #14725 ) ;
#22643 = ORIENTED_EDGE ( 'NONE', *, *, #21365, .T. ) ;
#22644 = CARTESIAN_POINT ( 'NONE',  ( 64.39795365981944997, -5.000000000000000888, 6.123233995736776143E-16 ) ) ;
#22645 = PLANE ( 'NONE',  #22725 ) ;
#22646 = EDGE_CURVE ( 'NONE', #12916, #780, #6014, .T. ) ;
#22647 = ORIENTED_EDGE ( 'NONE', *, *, #4369, .F. ) ;
#22648 = CARTESIAN_POINT ( 'NONE',  ( 5.871322893124551356, -8.081182679343980269, -7.759589141758143072 ) ) ;
#22649 = CARTESIAN_POINT ( 'NONE',  ( -5.622572944242077574E-13, 8.680847955711007202, 3.133165578109187610 ) ) ;
#22650 = DIRECTION ( 'NONE',  ( -0.000000000000000000, -0.000000000000000000, -1.000000000000000000 ) ) ;
#22651 = DIRECTION ( 'NONE',  ( -0.7052211081716895924, -0.7089874389501509278, 0.000000000000000000 ) ) ;
#22652 = CYLINDRICAL_SURFACE ( 'NONE', #6831, 4.499999999999997335 ) ;
#22653 = CARTESIAN_POINT ( 'NONE',  ( 5.365059087799947335, -7.384370330706356178, -12.33316557810918823 ) ) ;
#22654 = EDGE_CURVE ( 'NONE', #1008, #16958, #17745, .T. ) ;
#22655 = EDGE_LOOP ( 'NONE', ( #10922, #22388, #5719, #22435 ) ) ;
#22656 = ORIENTED_EDGE ( 'NONE', *, *, #23098, .F. ) ;
#22657 = CONICAL_SURFACE ( 'NONE', #3559, 1.999999999999996669, 1.029744258676653867 ) ;
#22658 = VECTOR ( 'NONE', #15296, 1000.000000000000000 ) ;
#22659 = AXIS2_PLACEMENT_3D ( 'NONE', #9908, #17366, #667 ) ;
#22660 = EDGE_LOOP ( 'NONE', ( #22579, #2978 ) ) ;
#22661 = ORIENTED_EDGE ( 'NONE', *, *, #11084, .T. ) ;
#22662 = CYLINDRICAL_SURFACE ( 'NONE', #600, 8.000000000000003553 ) ;
#22663 = LINE ( 'NONE', #5724, #4543 ) ;
#22664 = CARTESIAN_POINT ( 'NONE',  ( 23.90000000000000924, -29.50000000000000711, -27.00000000000000000 ) ) ;
#22665 = FACE_OUTER_BOUND ( 'NONE', #3734, .T. ) ;
#22666 = CARTESIAN_POINT ( 'NONE',  ( 65.85249911436491743, 7.562528597612068045E-15, 0.000000000000000000 ) ) ;
#22667 = DIRECTION ( 'NONE',  ( -0.000000000000000000, -0.000000000000000000, -1.000000000000000000 ) ) ;
#22668 = ADVANCED_FACE ( 'NONE', ( #9653 ), #6137, .F. ) ;
#22669 = DIRECTION ( 'NONE',  ( -0.000000000000000000, -0.000000000000000000, -1.000000000000000000 ) ) ;
#22670 = VERTEX_POINT ( 'NONE', #2347 ) ;
#22671 = MECHANICAL_DESIGN_GEOMETRIC_PRESENTATION_REPRESENTATION (  '', ( #16787 ), #11738 ) ;
#22672 = CIRCLE ( 'NONE', #6360, 0.6999999999999996225 ) ;
#22673 = EDGE_CURVE ( 'NONE', #15508, #20363, #8313, .T. ) ;
#22674 = CARTESIAN_POINT ( 'NONE',  ( 29.00000000000000000, 29.50000000000000000, -3.000000000000000000 ) ) ;
#22675 =( LENGTH_UNIT ( ) NAMED_UNIT ( * ) SI_UNIT ( .MILLI., .METRE. ) );
#22676 = DIRECTION ( 'NONE',  ( -1.000000000000000000, 0.000000000000000000, 0.000000000000000000 ) ) ;
#22677 = AXIS2_PLACEMENT_3D ( 'NONE', #8041, #16956, #270 ) ;
#22678 = DIRECTION ( 'NONE',  ( 1.000000000000000000, 0.000000000000000000, 0.000000000000000000 ) ) ;
#22679 = EDGE_LOOP ( 'NONE', ( #13215, #23453, #3662, #18754 ) ) ;
#22680 = CARTESIAN_POINT ( 'NONE',  ( 0.000000000000000000, 0.000000000000000000, 53.00000000000000000 ) ) ;
#22681 = ORIENTED_EDGE ( 'NONE', *, *, #6799, .F. ) ;
#22682 = EDGE_LOOP ( 'NONE', ( #2613, #8603, #18932, #9034 ) ) ;
#22683 = CARTESIAN_POINT ( 'NONE',  ( -7.685661446562381371, 5.583959896777970222, 8.859589141758144493 ) ) ;
#22684 = ORIENTED_EDGE ( 'NONE', *, *, #18204, .T. ) ;
#22685 =( NAMED_UNIT ( * ) SI_UNIT ( $, .STERADIAN. ) SOLID_ANGLE_UNIT ( ) );
#22686 = LINE ( 'NONE', #20270, #3680 ) ;
#22687 = DIRECTION ( 'NONE',  ( -1.000000000000000000, -1.224606353822377258E-16, -0.000000000000000000 ) ) ;
#22688 = AXIS2_PLACEMENT_3D ( 'NONE', #16675, #17030, #17145 ) ;
#22689 = VECTOR ( 'NONE', #20747, 1000.000000000000000 ) ;
#22690 = AXIS2_PLACEMENT_3D ( 'NONE', #21461, #6695, #12514 ) ;
#22691 = DIRECTION ( 'NONE',  ( -1.000000000000000000, -1.224606353822377258E-16, -0.000000000000000000 ) ) ;
#22692 = CIRCLE ( 'NONE', #15262, 8.999999999999998224 ) ;
#22693 = VECTOR ( 'NONE', #3180, 1000.000000000000000 ) ;
#22694 = DIRECTION ( 'NONE',  ( 0.000000000000000000, -1.000000000000000000, 0.000000000000000000 ) ) ;
#22695 = DIRECTION ( 'NONE',  ( -1.000000000000000000, 0.000000000000000000, 0.000000000000000000 ) ) ;
#22696 = CARTESIAN_POINT ( 'NONE',  ( 6.809999908187194197E-13, -9.988891130263535700, -3.559589141758143338 ) ) ;
#22697 = DIRECTION ( 'NONE',  ( 0.000000000000000000, 0.000000000000000000, 1.000000000000000000 ) ) ;
#22698 = ADVANCED_FACE ( 'NONE', ( #17101 ), #13313, .F. ) ;
#22699 = EDGE_CURVE ( 'NONE', #16900, #19190, #23978, .T. ) ;
#22700 = EDGE_LOOP ( 'NONE', ( #13879, #7545, #22945, #4123 ) ) ;
#22701 = LINE ( 'NONE', #21371, #21968 ) ;
#22702 = CARTESIAN_POINT ( 'NONE',  ( -9.377778780038873663, 0.5146052038006584395, 12.11160675903709816 ) ) ;
#22703 = AXIS2_PLACEMENT_3D ( 'NONE', #12152, #23415, #10198 ) ;
#22704 = FACE_BOUND ( 'NONE', #5521, .T. ) ;
#22705 = CIRCLE ( 'NONE', #7115, 5.000000000000007994 ) ;
#22706 = DIRECTION ( 'NONE',  ( 0.000000000000000000, -1.000000000000000000, 0.000000000000000000 ) ) ;
#22707 = AXIS2_PLACEMENT_3D ( 'NONE', #19643, #2918, #8259 ) ;
#22708 = DIRECTION ( 'NONE',  ( 0.000000000000000000, 1.000000000000000000, 0.000000000000000000 ) ) ;
#22709 = CONICAL_SURFACE ( 'NONE', #19613, 5.000000000000007994, 0.9599310885968855844 ) ;
#22710 = VECTOR ( 'NONE', #9130, 1000.000000000000114 ) ;
#22711 = DIRECTION ( 'NONE',  ( -1.000000000000000000, -1.224606353822377258E-16, -0.000000000000000000 ) ) ;
#22712 = CONICAL_SURFACE ( 'NONE', #15682, 5.000000000000007994, 0.9599310885968855844 ) ;
#22713 = CARTESIAN_POINT ( 'NONE',  ( -9.499999999999790390, -3.086737114213257804, -4.306742014460233747 ) ) ;
#22714 = ORIENTED_EDGE ( 'NONE', *, *, #2189, .F. ) ;
#22715 = CIRCLE ( 'NONE', #18058, 1.000000000000000888 ) ;
#22716 = DIRECTION ( 'NONE',  ( 0.000000000000000000, -1.000000000000000000, 0.000000000000000000 ) ) ;
#22717 = CARTESIAN_POINT ( 'NONE',  ( 8.680847955711007202, 5.912916378492122225E-13, 8.633165578109188942 ) ) ;
#22718 = AXIS2_PLACEMENT_3D ( 'NONE', #17498, #17613, #21301 ) ;
#22719 = DIRECTION ( 'NONE',  ( 2.600433232233976523E-16, 1.000000000000000000, 0.000000000000000000 ) ) ;
#22720 = DIRECTION ( 'NONE',  ( -1.000000000000000000, -0.000000000000000000, -0.000000000000000000 ) ) ;
#22721 = APPLICATION_CONTEXT ( 'automotive_design' ) ;
#22722 = ORIENTED_EDGE ( 'NONE', *, *, #17133, .F. ) ;
#22723 = EDGE_CURVE ( 'NONE', #5778, #10212, #16566, .T. ) ;
#22724 = VERTEX_POINT ( 'NONE', #4309 ) ;
#22725 = AXIS2_PLACEMENT_3D ( 'NONE', #15173, #8589, #10537 ) ;
#22726 = ITEM_DEFINED_TRANSFORMATION ( 'NONE', 'NONE', #10369,  #8005 ) ;
#22727 = ORIENTED_EDGE ( 'NONE', *, *, #1730, .T. ) ;
#22729 = CIRCLE ( 'NONE', #5975, 4.172000000000008590 ) ;
#22728 = DIRECTION ( 'NONE',  ( -1.000000000000000000, -0.000000000000000000, -0.000000000000000000 ) ) ;
#22730 = AXIS2_PLACEMENT_3D ( 'NONE', #20073, #19721, #5065 ) ;
#22731 = ADVANCED_FACE ( 'NONE', ( #2470 ), #6056, .F. ) ;
#22732 = CARTESIAN_POINT ( 'NONE',  ( 5.871322893124553133, -8.081182679343980269, -10.90674201446023339 ) ) ;
#22733 = ORIENTED_EDGE ( 'NONE', *, *, #8492, .T. ) ;
#22734 = ORIENTED_EDGE ( 'NONE', *, *, #22229, .T. ) ;
#22735 = AXIS2_PLACEMENT_3D ( 'NONE', #14415, #23822, #3094 ) ;
#22736 = EDGE_CURVE ( 'NONE', #10776, #12175, #4910, .T. ) ;
#22737 = EDGE_CURVE ( 'NONE', #22129, #8481, #21656, .T. ) ;
#22738 = DIRECTION ( 'NONE',  ( -0.000000000000000000, -0.000000000000000000, -1.000000000000000000 ) ) ;
#22739 = AXIS2_PLACEMENT_3D ( 'NONE', #3060, #18059, #6839 ) ;
#22740 = ORIENTED_EDGE ( 'NONE', *, *, #19498, .T. ) ;
#22741 = CARTESIAN_POINT ( 'NONE',  ( -5.279840276022249590, -7.916949377623846651, -3.501202454935721686 ) ) ;
#22742 = VERTEX_POINT ( 'NONE', #2604 ) ;
#22743 = FACE_OUTER_BOUND ( 'NONE', #14494, .T. ) ;
#22744 = CARTESIAN_POINT ( 'NONE',  ( 41.99999999999999289, 6.781874047275040887E-15, 9.499999999999987566 ) ) ;
#22745 = CARTESIAN_POINT ( 'NONE',  ( -31.74999999999995737, 0.000000000000000000, 5.000000000000000888 ) ) ;
#22746 = DIRECTION ( 'NONE',  ( 0.1039766011667100087, 0.9945797436152714610, 0.000000000000000000 ) ) ;
#22747 = ORIENTED_EDGE ( 'NONE', *, *, #22445, .T. ) ;
#22748 = AXIS2_PLACEMENT_3D ( 'NONE', #5991, #12062, #15742 ) ;
#22749 = LINE ( 'NONE', #16874, #19244 ) ;
#22750 = DIRECTION ( 'NONE',  ( -1.000000000000000000, 0.000000000000000000, 0.000000000000000000 ) ) ;
#22751 = ORIENTED_EDGE ( 'NONE', *, *, #13188, .F. ) ;
#22752 = AXIS2_PLACEMENT_3D ( 'NONE', #12356, #17979, #8075 ) ;
#22753 = ORIENTED_EDGE ( 'NONE', *, *, #21779, .T. ) ;
#22754 = CARTESIAN_POINT ( 'NONE',  ( 2.935661446562616295, -9.035036904803758873, 11.65958914175814520 ) ) ;
#22755 = ORIENTED_EDGE ( 'NONE', *, *, #8893, .T. ) ;
#22756 = CIRCLE ( 'NONE', #12602, 1.499999999999999778 ) ;
#22757 = ORIENTED_EDGE ( 'NONE', *, *, #21102, .F. ) ;
#22758 = CIRCLE ( 'NONE', #23539, 5.000000000000000888 ) ;
#22759 = LINE ( 'NONE', #6739, #11076 ) ;
#22760 = EDGE_CURVE ( 'NONE', #16878, #2783, #10014, .T. ) ;
#22761 = CIRCLE ( 'NONE', #8733, 5.000000000000007994 ) ;
#22762 = ORIENTED_EDGE ( 'NONE', *, *, #6631, .F. ) ;
#22763 = ORIENTED_EDGE ( 'NONE', *, *, #4525, .T. ) ;
#22764 = FACE_OUTER_BOUND ( 'NONE', #16983, .T. ) ;
#22765 = CARTESIAN_POINT ( 'NONE',  ( -5.622572944242076564E-13, 8.680847955711007202, -3.133165578109187166 ) ) ;
#22766 = CARTESIAN_POINT ( 'NONE',  ( 77.48886275072855767, 7.562528597612068045E-15, 0.000000000000000000 ) ) ;
#22767 = ORIENTED_EDGE ( 'NONE', *, *, #9368, .F. ) ;
#22768 = LINE ( 'NONE', #11633, #23932 ) ;
#22769 = CYLINDRICAL_SURFACE ( 'NONE', #6481, 4.249999999999996447 ) ;
#22770 = DIRECTION ( 'NONE',  ( -1.000000000000000000, 0.000000000000000000, 0.000000000000000000 ) ) ;
#22771 = EDGE_CURVE ( 'NONE', #6272, #704, #19918, .T. ) ;
#22772 = EDGE_CURVE ( 'NONE', #779, #4606, #21634, .T. ) ;
#22773 = DIRECTION ( 'NONE',  ( 0.000000000000000000, 0.000000000000000000, 1.000000000000000000 ) ) ;
#22774 = ORIENTED_EDGE ( 'NONE', *, *, #1836, .T. ) ;
#22775 = CARTESIAN_POINT ( 'NONE',  ( 41.00000000000000000, -6.000000000000015099, 12.00000000000000000 ) ) ;
#22776 = CONICAL_SURFACE ( 'NONE', #17312, 1.999999999999996669, 1.029744258676653867 ) ;
#22777 = ORIENTED_EDGE ( 'NONE', *, *, #3528, .F. ) ;
#22778 = CARTESIAN_POINT ( 'NONE',  ( 9.500000000000209610, -3.086737114211962396, -7.959589141758143249 ) ) ;
#22779 = CARTESIAN_POINT ( 'NONE',  ( -2.983080266967717442, 45.00000000000000000, 0.000000000000000000 ) ) ;
#22780 = AXIS2_PLACEMENT_3D ( 'NONE', #17970, #23358, #21394 ) ;
#22781 = CARTESIAN_POINT ( 'NONE',  ( 15.07341617659254496, 4.495283618570412365, -8.379779594489210837 ) ) ;
#22782 = AXIS2_PLACEMENT_3D ( 'NONE', #22419, #12998, #3972 ) ;
#22783 = DIRECTION ( 'NONE',  ( 0.000000000000000000, 1.000000000000000000, 0.000000000000000000 ) ) ;
#22784 = CARTESIAN_POINT ( 'NONE',  ( 0.000000000000000000, -9.374578970469700678, 10.68280860024311885 ) ) ;
#22785 = ORIENTED_EDGE ( 'NONE', *, *, #13105, .T. ) ;
#22786 = SURFACE_STYLE_FILL_AREA ( #2033 ) ;
#22787 = ORIENTED_EDGE ( 'NONE', *, *, #8879, .T. ) ;
#22788 = ORIENTED_EDGE ( 'NONE', *, *, #21425, .F. ) ;
#22789 = CARTESIAN_POINT ( 'NONE',  ( 7.022953521754877748, 5.102474405760673903, 10.83316557810919001 ) ) ;
#22790 = VERTEX_POINT ( 'NONE', #12342 ) ;
#22791 = DIRECTION ( 'NONE',  ( -3.285119681675809768E-17, -6.845718385068106880E-17, 0.9999999999999998890 ) ) ;
#22792 = CIRCLE ( 'NONE', #23960, 1.999999999999994449 ) ;
#22793 = CIRCLE ( 'NONE', #16150, 20.85000000000000142 ) ;
#22794 = ORIENTED_EDGE ( 'NONE', *, *, #216, .T. ) ;
#22795 = FACE_OUTER_BOUND ( 'NONE', #2612, .T. ) ;
#22796 = DIRECTION ( 'NONE',  ( 0.000000000000000000, 1.000000000000000000, 0.000000000000000000 ) ) ;
#22797 = UNCERTAINTY_MEASURE_WITH_UNIT (LENGTH_MEASURE( 1.000000000000000082E-05 ), #17906, 'distance_accuracy_value', 'NONE');
#22798 = AXIS2_PLACEMENT_3D ( 'NONE', #11535, #7505, #20590 ) ;
#22799 = AXIS2_PLACEMENT_3D ( 'NONE', #6204, #7887, #5839 ) ;
#22800 = CARTESIAN_POINT ( 'NONE',  ( 2.935661446562616295, -9.035036904803758873, -10.80674201446023197 ) ) ;
#22801 = CYLINDRICAL_SURFACE ( 'NONE', #7287, 5.000000000000000888 ) ;
#22802 = CARTESIAN_POINT ( 'NONE',  ( 5.871322893124551356, -8.081182679343980269, 6.906742014460233392 ) ) ;
#22803 = ADVANCED_FACE ( 'NONE', ( #16001 ), #8805, .T. ) ;
#22804 = ORIENTED_EDGE ( 'NONE', *, *, #10823, .F. ) ;
#22805 = CIRCLE ( 'NONE', #18126, 9.000000000000000000 ) ;
#22806 = AXIS2_PLACEMENT_3D ( 'NONE', #7302, #11061, #20487 ) ;
#22807 = CARTESIAN_POINT ( 'NONE',  ( 0.000000000000000000, -12.99147757894464306, 7.750000000000000000 ) ) ;
#22808 = CARTESIAN_POINT ( 'NONE',  ( -42.00000000000000000, -26.82133436441678853, 11.00000000000000000 ) ) ;
#22809 = ORIENTED_EDGE ( 'NONE', *, *, #6236, .T. ) ;
#22810 = CARTESIAN_POINT ( 'NONE',  ( -1.999999999999994449, 45.00000000000000000, -23.99999999999999645 ) ) ;
#22811 = FACE_OUTER_BOUND ( 'NONE', #10773, .T. ) ;
#22812 = CARTESIAN_POINT ( 'NONE',  ( -16.36153765883235423, 6.593687918952694460, -6.842832175870697142 ) ) ;
#22813 =( BOUNDED_CURVE ( )  B_SPLINE_CURVE ( 2, ( #8972, #23875, #7156, #14722, #22067, #12766, #22183, #697, #11758, #19111, #9938 ),
 .UNSPECIFIED., .F., .T. ) 
 B_SPLINE_CURVE_WITH_KNOTS ( ( 3, 2, 2, 2, 2, 3 ),
 ( 0.6000000000000000888, 0.6200000000000001066, 0.6400000000000001243, 0.6600000000000001421, 0.6800000000000001599, 0.7000000000000000666 ),
 .UNSPECIFIED. ) 
 CURVE ( )  GEOMETRIC_REPRESENTATION_ITEM ( )  RATIONAL_B_SPLINE_CURVE ( ( 0.9999999999999997780, 0.9510565162951537532, 1.000000000000000000, 0.9510565162951535312, 1.000000000000000000, 0.9510565162951535312, 1.000000000000000000, 0.9510565162951535312, 1.000000000000000000, 0.9510565162951533091, 1.000000000000000222 ) ) 
 REPRESENTATION_ITEM ( '' )  );
#22814 = CARTESIAN_POINT ( 'NONE',  ( -41.99999999999999289, 0.000000000000000000, 10.50249999999999950 ) ) ;
#22815 = ORIENTED_EDGE ( 'NONE', *, *, #1233, .F. ) ;
#22816 = TOROIDAL_SURFACE ( 'NONE', #11089, 6.500000000000000888, 1.500000000000000000 ) ;
#22817 = ORIENTED_EDGE ( 'NONE', *, *, #10862, .T. ) ;
#22818 = VECTOR ( 'NONE', #19285, 1000.000000000000000 ) ;
#22819 = ORIENTED_EDGE ( 'NONE', *, *, #20851, .F. ) ;
#22820 = CARTESIAN_POINT ( 'NONE',  ( 9.500000000000209610, -3.086737114211962396, 9.959589141758145914 ) ) ;
#22821 = CARTESIAN_POINT ( 'NONE',  ( 86.21613547800127719, -5.000000000000000888, 6.123233995736776143E-16 ) ) ;
#22822 = ADVANCED_FACE ( 'NONE', ( #17852 ), #16129, .F. ) ;
#22823 = CIRCLE ( 'NONE', #10763, 5.099999999999996980 ) ;
#22824 = ORIENTED_EDGE ( 'NONE', *, *, #13958, .T. ) ;
#22825 = VECTOR ( 'NONE', #18362, 1000.000000000000000 ) ;
#22826 = DIRECTION ( 'NONE',  ( 0.000000000000000000, 0.000000000000000000, 1.000000000000000000 ) ) ;
#22827 = CARTESIAN_POINT ( 'NONE',  ( 62.94340820527399671, 5.000000000000015987, 0.000000000000000000 ) ) ;
#22828 = DIRECTION ( 'NONE',  ( 0.000000000000000000, -0.000000000000000000, -1.000000000000000000 ) ) ;
#22829 = ORIENTED_EDGE ( 'NONE', *, *, #10044, .F. ) ;
#22830 = ADVANCED_FACE ( 'NONE', ( #10745 ), #23227, .T. ) ;
#22831 = CYLINDRICAL_SURFACE ( 'NONE', #15000, 9.500000000000000000 ) ;
#22832 = EDGE_CURVE ( 'NONE', #20166, #23563, #8399, .T. ) ;
#22833 = DIRECTION ( 'NONE',  ( 1.000000000000000000, 1.224606353822377258E-16, 0.000000000000000000 ) ) ;
#22834 = ADVANCED_FACE ( 'NONE', ( #5044 ), #23592, .F. ) ;
#22835 = VECTOR ( 'NONE', #5273, 1000.000000000000000 ) ;
#22836 = FACE_BOUND ( 'NONE', #9463, .T. ) ;
#22837 = EDGE_LOOP ( 'NONE', ( #8933, #12552, #22757, #21798 ) ) ;
#22838 = AXIS2_PLACEMENT_3D ( 'NONE', #3995, #20483, #1825 ) ;
#22839 = PLANE ( 'NONE',  #10589 ) ;
#22840 = CONICAL_SURFACE ( 'NONE', #22064, 5.000000000000007994, 0.9599310885968855844 ) ;
#22841 = EDGE_LOOP ( 'NONE', ( #1216, #18176 ) ) ;
#22842 = FACE_BOUND ( 'NONE', #7033, .T. ) ;
#22843 = DIRECTION ( 'NONE',  ( 0.5735764363510427177, -0.8191520442889941300, 1.003171929053527705E-16 ) ) ;
#22844 = DIRECTION ( 'NONE',  ( -1.000000000000000000, 0.000000000000000000, 0.000000000000000000 ) ) ;
#22845 = VECTOR ( 'NONE', #8955, 1000.000000000000000 ) ;
#22846 = DIRECTION ( 'NONE',  ( 1.000000000000000000, 0.000000000000000000, 0.000000000000000000 ) ) ;
#22847 = DIRECTION ( 'NONE',  ( 0.000000000000000000, 0.000000000000000000, 1.000000000000000000 ) ) ;
#22848 = DIRECTION ( 'NONE',  ( -0.7071067811865487940, -4.816422645751019675E-14, -0.7071067811865463515 ) ) ;
#22849 = LINE ( 'NONE', #13564, #1322 ) ;
#22850 = CARTESIAN_POINT ( 'NONE',  ( -5.871322893123450015, -8.081182679344781405, -4.506742014460231260 ) ) ;
#22851 = EDGE_LOOP ( 'NONE', ( #19148, #23584, #16140, #6624 ) ) ;
#22852 = DIRECTION ( 'NONE',  ( -1.000000000000000000, 0.000000000000000000, 0.000000000000000000 ) ) ;
#22853 = CARTESIAN_POINT ( 'NONE',  ( -2.682529543900285862, 8.255977015246234174, 7.233165578109188587 ) ) ;
#22854 = EDGE_CURVE ( 'NONE', #13831, #11194, #2964, .T. ) ;
#22855 = AXIS2_PLACEMENT_3D ( 'NONE', #18266, #8862, #14348 ) ;
#22856 = LINE ( 'NONE', #290, #12713 ) ;
#22857 = ORIENTED_EDGE ( 'NONE', *, *, #19604, .T. ) ;
#22858 = CIRCLE ( 'NONE', #19749, 1.999999999999994449 ) ;
#22859 = CARTESIAN_POINT ( 'NONE',  ( 2.879195777975148768E-17, 0.000000000000000000, 10.02592346138681023 ) ) ;
#22860 = EDGE_CURVE ( 'NONE', #12368, #20829, #17826, .T. ) ;
#22861 = EDGE_CURVE ( 'NONE', #20379, #16889, #17365, .T. ) ;
#22862 = VECTOR ( 'NONE', #3665, 1000.000000000000000 ) ;
#22863 = AXIS2_PLACEMENT_3D ( 'NONE', #22094, #12790, #5478 ) ;
#22864 = EDGE_LOOP ( 'NONE', ( #2735, #10603, #4426, #20452 ) ) ;
#22865 = ORIENTED_EDGE ( 'NONE', *, *, #17666, .T. ) ;
#22866 = CARTESIAN_POINT ( 'NONE',  ( 23.84999999999999432, -15.03999999999999559, 27.00000000000000000 ) ) ;
#22867 = CARTESIAN_POINT ( 'NONE',  ( 7.685661446562381371, -5.583959896777971110, -13.00674201446023304 ) ) ;
#22868 = ORIENTED_EDGE ( 'NONE', *, *, #15525, .T. ) ;
#22869 = VERTEX_POINT ( 'NONE', #3322 ) ;
#22870 = AXIS2_PLACEMENT_3D ( 'NONE', #8550, #23086, #10387 ) ;
#22871 = DIRECTION ( 'NONE',  ( 0.000000000000000000, 0.000000000000000000, 1.000000000000000000 ) ) ;
#22872 = EDGE_LOOP ( 'NONE', ( #953, #22615, #55, #23183, #19824 ) ) ;
#22873 = CARTESIAN_POINT ( 'NONE',  ( -3.828533837984870125, -8.711343052635822204, -3.501988579199554863 ) ) ;
#22874 = VERTEX_POINT ( 'NONE', #21865 ) ;
#22875 = CARTESIAN_POINT ( 'NONE',  ( 30.16774287754692807, 40.66994976491903913, -3.000000000000000000 ) ) ;
#22876 = CARTESIAN_POINT ( 'NONE',  ( 35.99999999999999289, 50.99999999999999289, 12.50000000000000000 ) ) ;
#22877 = LINE ( 'NONE', #11495, #9097 ) ;
#22878 = PRODUCT_DEFINITION_CONTEXT ( 'detailed design', #19315, 'design' ) ;
#22879 = CARTESIAN_POINT ( 'NONE',  ( -28.99999999999999645, -29.50000000000000000, -3.000000000000000000 ) ) ;
#22880 = ORIENTED_EDGE ( 'NONE', *, *, #2001, .F. ) ;
#22881 = CARTESIAN_POINT ( 'NONE',  ( 29.00000000000000000, 29.50000000000000355, 12.00000000000000000 ) ) ;
#22882 = CARTESIAN_POINT ( 'NONE',  ( -31.74999999999995737, 6.123233995736767268E-16, -5.000000000000000888 ) ) ;
#22883 = FACE_OUTER_BOUND ( 'NONE', #12736, .T. ) ;
#22884 = ORIENTED_EDGE ( 'NONE', *, *, #3237, .T. ) ;
#22885 = VECTOR ( 'NONE', #184, 1000.000000000000000 ) ;
#22886 = ORIENTED_EDGE ( 'NONE', *, *, #18761, .F. ) ;
#22887 = CARTESIAN_POINT ( 'NONE',  ( 6.222797240145152671E-13, -9.127583699786111282, 6.133165578109188942 ) ) ;
#22888 = EDGE_LOOP ( 'NONE', ( #15138, #14134, #23261, #8237 ) ) ;
#22889 = EDGE_CURVE ( 'NONE', #20146, #15114, #12677, .T. ) ;
#22890 = VERTEX_POINT ( 'NONE', #23353 ) ;
#22891 = EDGE_CURVE ( 'NONE', #15563, #9946, #20881, .T. ) ;
#22892 = VERTEX_POINT ( 'NONE', #12457 ) ;
#22893 = ORIENTED_EDGE ( 'NONE', *, *, #3941, .T. ) ;
#22894 = CARTESIAN_POINT ( 'NONE',  ( 41.50000000000000000, -28.80990663662250739, 0.000000000000000000 ) ) ;
#22895 = DIRECTION ( 'NONE',  ( 0.000000000000000000, 0.7557495743542551603, 0.6548607339452887643 ) ) ;
#22896 = EDGE_LOOP ( 'NONE', ( #13089, #17098, #21801, #22714, #21064 ) ) ;
#22897 = FACE_OUTER_BOUND ( 'NONE', #20480, .T. ) ;
#22898 = DIRECTION ( 'NONE',  ( 1.000000000000000000, 0.000000000000000000, 0.000000000000000000 ) ) ;
#22899 = CARTESIAN_POINT ( 'NONE',  ( 79.81818181818181301, 7.491529369508391930E-15, 0.000000000000000000 ) ) ;
#22900 = CARTESIAN_POINT ( 'NONE',  ( -31.74999999999995737, 0.000000000000000000, 5.000000000000000888 ) ) ;
#22901 = VERTEX_POINT ( 'NONE', #6512 ) ;
#22902 = DIRECTION ( 'NONE',  ( -1.000000000000000000, 0.000000000000000000, 0.000000000000000000 ) ) ;
#22903 = ORIENTED_EDGE ( 'NONE', *, *, #7669, .F. ) ;
#22904 = CARTESIAN_POINT ( 'NONE',  ( 5.871322893124551356, -8.081182679343980269, 3.759589141758144404 ) ) ;
#22905 = DIRECTION ( 'NONE',  ( 0.000000000000000000, 0.000000000000000000, -1.000000000000000000 ) ) ;
#22906 = DIRECTION ( 'NONE',  ( 0.5735764363510427177, -0.8191520442889941300, 1.003171929053527705E-16 ) ) ;
#22907 = EDGE_CURVE ( 'NONE', #13474, #5422, #23462, .T. ) ;
#22908 = DIRECTION ( 'NONE',  ( -1.000000000000000000, 0.000000000000000000, 0.000000000000000000 ) ) ;
#22909 = CARTESIAN_POINT ( 'NONE',  ( 8.680847955711199049, -2.820578480813074496, -6.533165578109188409 ) ) ;
#22910 = EDGE_CURVE ( 'NONE', #6894, #14074, #22057, .T. ) ;
#22911 = CARTESIAN_POINT ( 'NONE',  ( 85.05659179472598908, 5.000000000000025757, 6.123233995736788962E-16 ) ) ;
#22912 = EDGE_LOOP ( 'NONE', ( #23792, #21531, #4682, #8045, #2628 ) ) ;
#22913 = EDGE_LOOP ( 'NONE', ( #20883, #17721, #5895, #2116 ) ) ;
#22914 = CARTESIAN_POINT ( 'NONE',  ( 7.022953521755574080, -5.102474405759714671, 12.43316557810918788 ) ) ;
#22915 = EDGE_CURVE ( 'NONE', #5565, #17524, #14059, .T. ) ;
#22916 = EDGE_CURVE ( 'NONE', #12918, #17625, #23993, .T. ) ;
#22917 = ORIENTED_EDGE ( 'NONE', *, *, #21639, .F. ) ;
#22918 = DIRECTION ( 'NONE',  ( -0.1165783874715181911, -0.9931814937736913596, -5.309704129305497828E-16 ) ) ;
#22919 = CARTESIAN_POINT ( 'NONE',  ( 74.00000000000001421, 4.172000000000015696, 5.109226446042767468E-16 ) ) ;
#22920 = ORIENTED_EDGE ( 'NONE', *, *, #15079, .T. ) ;
#22921 = DIRECTION ( 'NONE',  ( 0.5735764363510427177, -0.8191520442889941300, 1.003171929053527705E-16 ) ) ;
#22922 = CARTESIAN_POINT ( 'NONE',  ( 9.500000000000000000, 6.470877716354879437E-13, -10.05958914175814378 ) ) ;
#22923 = CARTESIAN_POINT ( 'NONE',  ( 74.57977184163763695, 7.562528597612068045E-15, 0.000000000000000000 ) ) ;
#22924 = CARTESIAN_POINT ( 'NONE',  ( 41.73082370883257397, -27.62204025492843940, 0.000000000000000000 ) ) ;
#22925 = CARTESIAN_POINT ( 'NONE',  ( 2.935661446562616295, -9.035036904803758873, 6.806742014460233747 ) ) ;
#22926 = EDGE_LOOP ( 'NONE', ( #21073, #17229, #11328, #4423 ) ) ;
#22927 = CARTESIAN_POINT ( 'NONE',  ( 9.999999999999998224, 1.224646799147353059E-15, 0.000000000000000000 ) ) ;
#22928 = DIRECTION ( 'NONE',  ( -1.000000000000000000, -0.000000000000000000, -0.000000000000000000 ) ) ;
#22929 = CARTESIAN_POINT ( 'NONE',  ( 20.84999999999999432, -15.04000000000000448, 25.00000000000000000 ) ) ;
#22930 = VERTEX_POINT ( 'NONE', #14294 ) ;
#22931 = DIRECTION ( 'NONE',  ( 0.000000000000000000, 0.000000000000000000, 1.000000000000000000 ) ) ;
#22932 = DIRECTION ( 'NONE',  ( -0.000000000000000000, -0.000000000000000000, -1.000000000000000000 ) ) ;
#22933 = CARTESIAN_POINT ( 'NONE',  ( -16.19099482616364938, 6.271157271432195479, 7.149633965064785990 ) ) ;
#22934 = CIRCLE ( 'NONE', #18641, 5.100000000000000533 ) ;
#22935 = ADVANCED_FACE ( 'NONE', ( #21754 ), #19130, .T. ) ;
#22936 = CARTESIAN_POINT ( 'NONE',  ( 0.000000000000000000, 0.000000000000000000, 15.50000000000000000 ) ) ;
#22937 = CARTESIAN_POINT ( 'NONE',  ( -5.365059087799947335, 7.384370330706355290, -7.333165578109188232 ) ) ;
#22938 = CIRCLE ( 'NONE', #12401, 5.000000000000007994 ) ;
#22939 = AXIS2_PLACEMENT_3D ( 'NONE', #8813, #8455, #16831 ) ;
#22940 = VERTEX_POINT ( 'NONE', #13258 ) ;
#22941 = ORIENTED_EDGE ( 'NONE', *, *, #19250, .T. ) ;
#22942 = DIRECTION ( 'NONE',  ( 0.000000000000000000, -1.000000000000000000, 0.000000000000000000 ) ) ;
#22943 = CARTESIAN_POINT ( 'NONE',  ( -2.935661446561384391, -9.035036904804158553, 12.60674201446023446 ) ) ;
#22944 = ADVANCED_FACE ( 'NONE', ( #14655 ), #10855, .F. ) ;
#22945 = ORIENTED_EDGE ( 'NONE', *, *, #17660, .T. ) ;
#22946 = CYLINDRICAL_SURFACE ( 'NONE', #13798, 5.000000000000000888 ) ;
#22947 = CARTESIAN_POINT ( 'NONE',  ( -39.00000000000000000, -28.80990663662251450, 11.00000000000000000 ) ) ;
#22948 = FACE_OUTER_BOUND ( 'NONE', #17097, .T. ) ;
#22949 = DIRECTION ( 'NONE',  ( -0.000000000000000000, -0.000000000000000000, -1.000000000000000000 ) ) ;
#22950 = DIRECTION ( 'NONE',  ( -1.000000000000000000, 0.000000000000000000, 0.000000000000000000 ) ) ;
#22951 = DIRECTION ( 'NONE',  ( -1.000000000000000000, 0.000000000000000000, 0.000000000000000000 ) ) ;
#22952 =( BOUNDED_CURVE ( )  B_SPLINE_CURVE ( 2, ( #2988, #21770, #7232, #21880, #3337, #3097, #20179, #10519, #1271, #3458, #10760 ),
 .UNSPECIFIED., .F., .T. ) 
 B_SPLINE_CURVE_WITH_KNOTS ( ( 3, 2, 2, 2, 2, 3 ),
 ( 0.3000000000000000999, 0.3200000000000001177, 0.3400000000000000799, 0.3600000000000000422, 0.3800000000000000044, 0.4000000000000000222 ),
 .UNSPECIFIED. ) 
 CURVE ( )  GEOMETRIC_REPRESENTATION_ITEM ( )  RATIONAL_B_SPLINE_CURVE ( ( 0.9999999999999997780, 0.9510565162951537532, 1.000000000000000000, 0.9510565162951535312, 1.000000000000000000, 0.9510565162951535312, 1.000000000000000000, 0.9510565162951535312, 1.000000000000000000, 0.9510565162951535312, 1.000000000000000000 ) ) 
 REPRESENTATION_ITEM ( '' )  );
#22953 = DIRECTION ( 'NONE',  ( 0.000000000000000000, -1.000000000000000000, 0.000000000000000000 ) ) ;
#22954 = ORIENTED_EDGE ( 'NONE', *, *, #9148, .T. ) ;
#22955 = DIRECTION ( 'NONE',  ( -0.000000000000000000, 0.000000000000000000, -1.000000000000000000 ) ) ;
#22956 = ORIENTED_EDGE ( 'NONE', *, *, #20392, .F. ) ;
#22957 = CARTESIAN_POINT ( 'NONE',  ( 0.2186765406003783607, -9.110087292425127714, 12.42023503934770901 ) ) ;
#22958 = LINE ( 'NONE', #865, #7117 ) ;
#22959 = PLANE ( 'NONE',  #13575 ) ;
#22960 = DIRECTION ( 'NONE',  ( -0.000000000000000000, -0.000000000000000000, -1.000000000000000000 ) ) ;
#22961 = EDGE_CURVE ( 'NONE', #3419, #13300, #21990, .T. ) ;
#22962 = CARTESIAN_POINT ( 'NONE',  ( 9.500000000000000000, 1.163414459189985485E-15, 12.50000000000000000 ) ) ;
#22963 = CARTESIAN_POINT ( 'NONE',  ( 30.44534269664589843, 40.40463133211081015, 27.00000000000000000 ) ) ;
#22964 = CARTESIAN_POINT ( 'NONE',  ( -31.10231664966676846, 45.36128193761570770, 12.00000000000000000 ) ) ;
#22965 = ORIENTED_EDGE ( 'NONE', *, *, #19666, .T. ) ;
#22966 = CARTESIAN_POINT ( 'NONE',  ( -6.153822176767817416E-13, 9.500000000000000000, -3.706742014460232326 ) ) ;
#22967 = ORIENTED_EDGE ( 'NONE', *, *, #2456, .T. ) ;
#22968 = CARTESIAN_POINT ( 'NONE',  ( 0.000000000000000000, 0.000000000000000000, 0.000000000000000000 ) ) ;
#22969 = EDGE_CURVE ( 'NONE', #3902, #4778, #4253, .T. ) ;
#22970 = CARTESIAN_POINT ( 'NONE',  ( 8.680847955711199049, -2.820578480813074496, 6.533165578109188409 ) ) ;
#22971 = EDGE_CURVE ( 'NONE', #13127, #1485, #16929, .T. ) ;
#22972 = DIRECTION ( 'NONE',  ( 0.000000000000000000, -1.000000000000000000, 0.000000000000000000 ) ) ;
#22973 = CARTESIAN_POINT ( 'NONE',  ( 5.000000000000000000, 4.685197434473818312, -1.301042606982605321E-15 ) ) ;
#22974 = ORIENTED_EDGE ( 'NONE', *, *, #4467, .T. ) ;
#22975 = ORIENTED_EDGE ( 'NONE', *, *, #8875, .F. ) ;
#22976 = EDGE_LOOP ( 'NONE', ( #20539, #2296, #204 ) ) ;
#22977 = CYLINDRICAL_SURFACE ( 'NONE', #3718, 9.499999999999987566 ) ;
#22978 = CARTESIAN_POINT ( 'NONE',  ( 9.500000000000209610, -3.086737114211962396, -13.10674201446023091 ) ) ;
#22979 = ORIENTED_EDGE ( 'NONE', *, *, #11528, .T. ) ;
#22980 = VECTOR ( 'NONE', #10663, 1000.000000000000000 ) ;
#22981 = EDGE_CURVE ( 'NONE', #14475, #21066, #238, .T. ) ;
#22982 = CARTESIAN_POINT ( 'NONE',  ( 0.000000000000000000, 0.000000000000000000, 0.2999999999999990452 ) ) ;
#22983 = ORIENTED_EDGE ( 'NONE', *, *, #24077, .F. ) ;
#22984 = CARTESIAN_POINT ( 'NONE',  ( -9.122155368748954274, -2.709684805614216430, -3.500412170903221654 ) ) ;
#22985 = EDGE_CURVE ( 'NONE', #13101, #8857, #20168, .T. ) ;
#22986 = ORIENTED_EDGE ( 'NONE', *, *, #21, .F. ) ;
#22987 = CYLINDRICAL_SURFACE ( 'NONE', #16427, 5.000000000000000888 ) ;
#22988 = LINE ( 'NONE', #22744, #3987 ) ;
#22989 = CARTESIAN_POINT ( 'NONE',  ( -35.99999999999995026, 59.99999999999998579, 12.50000000000000000 ) ) ;
#22990 = CARTESIAN_POINT ( 'NONE',  ( -2.999999999999999112, 8.485281374238567764, 80.99999999999998579 ) ) ;
#22991 = VERTEX_POINT ( 'NONE', #11659 ) ;
#22992 = DIRECTION ( 'NONE',  ( 0.000000000000000000, 0.000000000000000000, -1.000000000000000000 ) ) ;
#22993 = DIRECTION ( 'NONE',  ( 1.000000000000000000, -2.600433232233976523E-16, 0.000000000000000000 ) ) ;
#22994 = DIRECTION ( 'NONE',  ( 0.000000000000000000, 0.000000000000000000, 1.000000000000000000 ) ) ;
#22995 = VERTEX_POINT ( 'NONE', #17164 ) ;
#22996 = EDGE_LOOP ( 'NONE', ( #6493, #22777 ) ) ;
#22997 = CARTESIAN_POINT ( 'NONE',  ( 5.871322893123449127, 8.081182679344781405, 8.359589141758144493 ) ) ;
#22998 = VERTEX_POINT ( 'NONE', #1607 ) ;
#22999 = AXIS2_PLACEMENT_3D ( 'NONE', #12436, #19538, #14156 ) ;
#23000 = VERTEX_POINT ( 'NONE', #7647 ) ;
#23001 = EDGE_LOOP ( 'NONE', ( #11174, #10018, #14932, #13628 ) ) ;
#23002 = ORIENTED_EDGE ( 'NONE', *, *, #14597, .F. ) ;
#23003 = VERTEX_POINT ( 'NONE', #3443 ) ;
#23004 = CARTESIAN_POINT ( 'NONE',  ( 8.680847955711199049, -2.820578480813074496, -6.533165578109188409 ) ) ;
#23005 = CARTESIAN_POINT ( 'NONE',  ( -7.685661446562381371, 5.583959896777970222, 8.006742014460233037 ) ) ;
#23006 = ORIENTED_EDGE ( 'NONE', *, *, #12675, .F. ) ;
#23007 = CARTESIAN_POINT ( 'NONE',  ( 62.94340820527399671, 7.562528597612068045E-15, 0.000000000000000000 ) ) ;
#23008 = CARTESIAN_POINT ( 'NONE',  ( -28.99999999999999645, 29.50000000000000000, -2.224999999999995204 ) ) ;
#23009 = DIRECTION ( 'NONE',  ( 0.5735764363510424957, 0.8191520442889943521, 0.000000000000000000 ) ) ;
#23010 = CARTESIAN_POINT ( 'NONE',  ( 3.934052222107095265, -8.094642247421083070, 12.50000000000000000 ) ) ;
#23011 = VERTEX_POINT ( 'NONE', #11419 ) ;
#23012 = DIRECTION ( 'NONE',  ( -1.000000000000000000, -0.000000000000000000, -0.000000000000000000 ) ) ;
#23013 = CARTESIAN_POINT ( 'NONE',  ( 44.99999999999998579, 50.99999999999992184, 12.50000000000000000 ) ) ;
#23014 = ADVANCED_FACE ( 'NONE', ( #8915 ), #22801, .T. ) ;
#23015 = EDGE_CURVE ( 'NONE', #10096, #13428, #22553, .T. ) ;
#23016 = EDGE_LOOP ( 'NONE', ( #3069, #9035, #5154, #2283 ) ) ;
#23017 = CARTESIAN_POINT ( 'NONE',  ( 0.000000000000000000, -15.23000000000000220, 27.00000000000000000 ) ) ;
#23018 = CARTESIAN_POINT ( 'NONE',  ( 76.03431729618309021, 7.562528597612068045E-15, 0.000000000000000000 ) ) ;
#23019 = LINE ( 'NONE', #4492, #18118 ) ;
#23020 = CARTESIAN_POINT ( 'NONE',  ( -7.022953521755574080, 5.102474405759713783, -5.433165578109188765 ) ) ;
#23021 = CARTESIAN_POINT ( 'NONE',  ( -28.99999999999999645, -29.50000000000001066, 27.00000000000000000 ) ) ;
#23022 = ORIENTED_EDGE ( 'NONE', *, *, #3129, .T. ) ;
#23023 = ORIENTED_EDGE ( 'NONE', *, *, #5985, .F. ) ;
#23024 = CARTESIAN_POINT ( 'NONE',  ( -8.680847955710813579, -2.820578480814258437, 9.733165578109186811 ) ) ;
#23025 = ORIENTED_EDGE ( 'NONE', *, *, #9581, .T. ) ;
#23026 = CARTESIAN_POINT ( 'NONE',  ( 70.21613547800127719, 7.562528597612068045E-15, 0.000000000000000000 ) ) ;
#23027 = PRESENTATION_LAYER_ASSIGNMENT (  '', '', ( #13665 ) ) ;
#23028 = ORIENTED_EDGE ( 'NONE', *, *, #13022, .F. ) ;
#23029 = CARTESIAN_POINT ( 'NONE',  ( 0.000000000000000000, 45.00000000000000000, 27.00000000000000000 ) ) ;
#23030 = DIRECTION ( 'NONE',  ( -1.000000000000000000, -1.224606353822377258E-16, -0.000000000000000000 ) ) ;
#23031 = UNCERTAINTY_MEASURE_WITH_UNIT (LENGTH_MEASURE( 1.000000000000000082E-05 ), #5012, 'distance_accuracy_value', 'NONE');
#23032 = ADVANCED_FACE ( 'NONE', ( #18323 ), #8456, .F. ) ;
#23033 = DIRECTION ( 'NONE',  ( 0.000000000000000000, 0.000000000000000000, 1.000000000000000000 ) ) ;
#23034 = CARTESIAN_POINT ( 'NONE',  ( -1.504652183083727168, 9.499999999999904077, 3.757996296007079184 ) ) ;
#23035 = CARTESIAN_POINT ( 'NONE',  ( -43.50000000000000711, 25.22443390181683043, -1.500000000000000000 ) ) ;
#23036 = EDGE_LOOP ( 'NONE', ( #11277, #21009, #7058, #753, #5635, #11740 ) ) ;
#23037 = CARTESIAN_POINT ( 'NONE',  ( -41.99999999999996447, -25.22443390181684464, -0.6213203435596427182 ) ) ;
#23038 = ADVANCED_FACE ( 'NONE', ( #14527 ), #5950, .F. ) ;
#23039 = CARTESIAN_POINT ( 'NONE',  ( 0.000000000000000000, 0.000000000000000000, 12.50000000000000000 ) ) ;
#23040 = EDGE_CURVE ( 'NONE', #4470, #23775, #11552, .T. ) ;
#23041 = CARTESIAN_POINT ( 'NONE',  ( -34.00000000000000000, -3.999999999999999112, 9.500000000000000000 ) ) ;
#23042 = EDGE_CURVE ( 'NONE', #7111, #1863, #21669, .T. ) ;
#23043 = ORIENTED_EDGE ( 'NONE', *, *, #5193, .F. ) ;
#23044 = DIRECTION ( 'NONE',  ( 0.000000000000000000, 0.000000000000000000, 1.000000000000000000 ) ) ;
#23045 = DIRECTION ( 'NONE',  ( -0.000000000000000000, -0.000000000000000000, -1.000000000000000000 ) ) ;
#23046 = CARTESIAN_POINT ( 'NONE',  ( -16.36913330654532217, 6.602951766536808265, 6.845624079409805773 ) ) ;
#23047 = DIRECTION ( 'NONE',  ( -1.000000000000000000, -1.224606353822377258E-16, -0.000000000000000000 ) ) ;
#23048 = ORIENTED_EDGE ( 'NONE', *, *, #2298, .F. ) ;
#23049 = CARTESIAN_POINT ( 'NONE',  ( -5.365059087798939252, -7.384370330707086261, -5.933165578109187877 ) ) ;
#23050 = CIRCLE ( 'NONE', #16395, 6.050000000006053646 ) ;
#23051 = ORIENTED_EDGE ( 'NONE', *, *, #11239, .T. ) ;
#23052 = CARTESIAN_POINT ( 'NONE',  ( 6.809999908187194197E-13, -9.988891130263535700, 11.55958914175814201 ) ) ;
#23053 = DIRECTION ( 'NONE',  ( 0.000000000000000000, -0.2817325568414366654, 0.9594929736144953702 ) ) ;
#23054 = ORIENTED_EDGE ( 'NONE', *, *, #15449, .T. ) ;
#23055 = CARTESIAN_POINT ( 'NONE',  ( 5.365059087799946447, -7.384370330706356178, -12.33316557810918646 ) ) ;
#23056 = DIRECTION ( 'NONE',  ( -1.000000000000000000, -1.224606353822377258E-16, -0.000000000000000000 ) ) ;
#23057 = EDGE_CURVE ( 'NONE', #12524, #910, #9711, .T. ) ;
#23058 = AXIS2_PLACEMENT_3D ( 'NONE', #17804, #12157, #2915 ) ;
#23059 = CARTESIAN_POINT ( 'NONE',  ( 7.121611749575429862, -5.132745777193602699, -12.49999999999999289 ) ) ;
#23060 = CARTESIAN_POINT ( 'NONE',  ( 0.000000000000000000, 5.985147671565707483, 12.89120389306417103 ) ) ;
#23061 = DIRECTION ( 'NONE',  ( 0.000000000000000000, -1.000000000000000000, 0.000000000000000000 ) ) ;
#23062 = AXIS2_PLACEMENT_3D ( 'NONE', #12971, #8844, #12848 ) ;
#23063 = CARTESIAN_POINT ( 'NONE',  ( 9.500000000000000000, 6.470877716354879437E-13, -4.059589141758143782 ) ) ;
#23064 = EDGE_LOOP ( 'NONE', ( #18983, #7514, #9899, #3177 ) ) ;
#23065 = DIRECTION ( 'NONE',  ( -1.000000000000000000, 0.000000000000000000, 0.000000000000000000 ) ) ;
#23066 = ADVANCED_FACE ( 'NONE', ( #22665 ), #11556, .T. ) ;
#23067 = EDGE_CURVE ( 'NONE', #5909, #4920, #3019, .T. ) ;
#23068 = ORIENTED_EDGE ( 'NONE', *, *, #14404, .F. ) ;
#23069 = CYLINDRICAL_SURFACE ( 'NONE', #15219, 5.000000000000004441 ) ;
#23070 = DIRECTION ( 'NONE',  ( 0.000000000000000000, 0.000000000000000000, 1.000000000000000000 ) ) ;
#23071 = DIRECTION ( 'NONE',  ( 0.5735764363510424957, 0.8191520442889943521, 0.000000000000000000 ) ) ;
#23072 = LINE ( 'NONE', #13799, #7775 ) ;
#23073 = ORIENTED_EDGE ( 'NONE', *, *, #23162, .T. ) ;
#23074 = CARTESIAN_POINT ( 'NONE',  ( -36.00000000000000711, -51.00000000000000711, 12.50000000000000000 ) ) ;
#23075 = CARTESIAN_POINT ( 'NONE',  ( 20.85000000000000853, 15.03999999999999915, -25.00000000000000000 ) ) ;
#23076 = EDGE_LOOP ( 'NONE', ( #7248, #424, #20773, #2956, #15611 ) ) ;
#23077 = CARTESIAN_POINT ( 'NONE',  ( 5.871322893124553133, -8.081182679343980269, -4.906742014460232504 ) ) ;
#23078 = VECTOR ( 'NONE', #11039, 1000.000000000000000 ) ;
#23079 = VERTEX_POINT ( 'NONE', #595 ) ;
#23080 = VECTOR ( 'NONE', #10781, 1000.000000000000227 ) ;
#23081 = DIRECTION ( 'NONE',  ( -1.000000000000000000, -0.000000000000000000, -0.000000000000000000 ) ) ;
#23082 = CARTESIAN_POINT ( 'NONE',  ( -7.022953521755574080, 5.102474405759713783, 7.433165578109188765 ) ) ;
#23083 = AXIS2_PLACEMENT_3D ( 'NONE', #7695, #2342, #520 ) ;
#23084 = CIRCLE ( 'NONE', #5939, 5.000000000000007994 ) ;
#23085 = AXIS2_PLACEMENT_3D ( 'NONE', #6637, #19335, #10409 ) ;
#23086 = DIRECTION ( 'NONE',  ( -1.000000000000000000, -1.224606353822377258E-16, -0.000000000000000000 ) ) ;
#23087 = AXIS2_PLACEMENT_3D ( 'NONE', #14414, #13961, #1038 ) ;
#23088 = DIRECTION ( 'NONE',  ( -0.000000000000000000, -0.000000000000000000, 1.000000000000000000 ) ) ;
#23089 = EDGE_LOOP ( 'NONE', ( #8002, #20577, #17681, #23726 ) ) ;
#23090 = CONTEXT_DEPENDENT_SHAPE_REPRESENTATION ( #18371, #3812 ) ;
#23091 = VERTEX_POINT ( 'NONE', #17654 ) ;
#23092 = DIRECTION ( 'NONE',  ( 0.000000000000000000, 0.000000000000000000, 1.000000000000000000 ) ) ;
#23093 = CARTESIAN_POINT ( 'NONE',  ( -5.871322893123450015, -8.081182679344781405, -12.50674201446023481 ) ) ;
#23094 = ORIENTED_EDGE ( 'NONE', *, *, #4338, .T. ) ;
#23095 = VECTOR ( 'NONE', #4994, 1000.000000000000000 ) ;
#23096 = CONICAL_SURFACE ( 'NONE', #12557, 1.999999999999994449, 1.029744258676653201 ) ;
#23097 = VECTOR ( 'NONE', #7531, 1000.000000000000000 ) ;
#23098 = EDGE_CURVE ( 'NONE', #17902, #3993, #14118, .T. ) ;
#23099 = LINE ( 'NONE', #17590, #17039 ) ;
#23100 = AXIS2_PLACEMENT_3D ( 'NONE', #18897, #23384, #19470 ) ;
#23101 = VERTEX_POINT ( 'NONE', #15698 ) ;
#23102 = TOROIDAL_SURFACE ( 'NONE', #1683, 2.000000000000000000, 1.000000000000000000 ) ;
#23103 = CIRCLE ( 'NONE', #12964, 1.500000000000001332 ) ;
#23104 = ORIENTED_EDGE ( 'NONE', *, *, #135, .T. ) ;
#23105 = DIRECTION ( 'NONE',  ( -1.000000000000000000, -1.224606353822377258E-16, -0.000000000000000000 ) ) ;
#23106 = CIRCLE ( 'NONE', #19200, 6.050000000006050982 ) ;
#23107 = CARTESIAN_POINT ( 'NONE',  ( 58.00000000000000000, 4.172000000000015696, 5.109226446042767468E-16 ) ) ;
#23108 = CARTESIAN_POINT ( 'NONE',  ( 33.25000000000000000, -29.50000000000000000, -2.224999999999995204 ) ) ;
#23109 = PRODUCT_DEFINITION_CONTEXT ( 'detailed design', #2636, 'design' ) ;
#23110 = DIRECTION ( 'NONE',  ( -0.000000000000000000, -0.000000000000000000, -1.000000000000000000 ) ) ;
#23111 = EDGE_LOOP ( 'NONE', ( #10107, #22548, #17325, #19555 ) ) ;
#23112 = CARTESIAN_POINT ( 'NONE',  ( -39.49999999999998579, 15.50000000000000000, 19.70000000000000284 ) ) ;
#23113 = DIRECTION ( 'NONE',  ( -1.000000000000000000, 0.000000000000000000, 0.000000000000000000 ) ) ;
#23114 = DIRECTION ( 'NONE',  ( 0.000000000000000000, 0.000000000000000000, 1.000000000000000000 ) ) ;
#23115 = ORIENTED_EDGE ( 'NONE', *, *, #20014, .T. ) ;
#23116 = ORIENTED_EDGE ( 'NONE', *, *, #135, .F. ) ;
#23117 = CARTESIAN_POINT ( 'NONE',  ( -7.685661446561619314, -5.583959896779019161, 9.259589141758143072 ) ) ;
#23118 = ORIENTED_EDGE ( 'NONE', *, *, #18306, .F. ) ;
#23119 = AXIS2_PLACEMENT_3D ( 'NONE', #5640, #151, #4041 ) ;
#23120 = ORIENTED_EDGE ( 'NONE', *, *, #10720, .T. ) ;
#23121 = VECTOR ( 'NONE', #21936, 1000.000000000000000 ) ;
#23122 = ORIENTED_EDGE ( 'NONE', *, *, #1857, .F. ) ;
#23123 = EDGE_CURVE ( 'NONE', #3216, #15508, #8012, .T. ) ;
#23124 = AXIS2_PLACEMENT_3D ( 'NONE', #1982, #3573, #15140 ) ;
#23125 = AXIS2_PLACEMENT_3D ( 'NONE', #13338, #3840, #22161 ) ;
#23126 = CIRCLE ( 'NONE', #8303, 5.000000000000007994 ) ;
#23127 = EDGE_LOOP ( 'NONE', ( #11198, #18149, #14109, #776 ) ) ;
#23128 = EDGE_CURVE ( 'NONE', #17902, #4813, #20727, .T. ) ;
#23129 = ORIENTED_EDGE ( 'NONE', *, *, #14060, .T. ) ;
#23130 = DIRECTION ( 'NONE',  ( 1.000000000000000000, 0.000000000000000000, 0.000000000000000000 ) ) ;
#23131 = CARTESIAN_POINT ( 'NONE',  ( 0.000000000000000000, 0.000000000000000000, 53.00000000000000000 ) ) ;
#23132 = AXIS2_PLACEMENT_3D ( 'NONE', #13660, #4169, #22694 ) ;
#23133 = DIRECTION ( 'NONE',  ( 1.000000000000000000, 0.000000000000000000, 0.000000000000000000 ) ) ;
#23134 = CARTESIAN_POINT ( 'NONE',  ( 0.000000000000000000, 0.000000000000000000, 0.000000000000000000 ) ) ;
#23135 = VERTEX_POINT ( 'NONE', #22924 ) ;
#23136 = CARTESIAN_POINT ( 'NONE',  ( -17.49066032632880763, -9.200828712690862332, 2.414248458042551615 ) ) ;
#23137 = DIRECTION ( 'NONE',  ( -0.000000000000000000, -0.000000000000000000, -1.000000000000000000 ) ) ;
#23138 = CARTESIAN_POINT ( 'NONE',  ( 9.500000000000000000, 6.470877716354879437E-13, -5.206742014460234103 ) ) ;
#23139 = ADVANCED_FACE ( 'NONE', ( #23412 ), #11916, .T. ) ;
#23140 = CYLINDRICAL_SURFACE ( 'NONE', #8929, 9.500000000000000000 ) ;
#23141 = ORIENTED_EDGE ( 'NONE', *, *, #4655, .F. ) ;
#23142 = CARTESIAN_POINT ( 'NONE',  ( -2.935661446561384391, -9.035036904804158553, 7.459589141758144137 ) ) ;
#23143 = VECTOR ( 'NONE', #22106, 1000.000000000000000 ) ;
#23144 = EDGE_LOOP ( 'NONE', ( #15879, #1858, #20986, #9765 ) ) ;
#23145 = CARTESIAN_POINT ( 'NONE',  ( -9.500000000000000000, -6.482511860946779655E-13, 5.059589141758143782 ) ) ;
#23146 = AXIS2_PLACEMENT_3D ( 'NONE', #9411, #13333, #15042 ) ;
#23147 = CIRCLE ( 'NONE', #7519, 14.42592346043842255 ) ;
#23148 = CARTESIAN_POINT ( 'NONE',  ( 17.06033556854817590, -8.068938288216797261, 5.036196554528626024 ) ) ;
#23149 = CONICAL_SURFACE ( 'NONE', #16884, 5.000000000000007994, 0.9599310885968855844 ) ;
#23150 = AXIS2_PLACEMENT_3D ( 'NONE', #10282, #12355, #12093 ) ;
#23151 = CYLINDRICAL_SURFACE ( 'NONE', #21980, 11.23082370883260417 ) ;
#23152 = AXIS2_PLACEMENT_3D ( 'NONE', #3590, #11010, #7260 ) ;
#23153 = CARTESIAN_POINT ( 'NONE',  ( 6.222797240145152671E-13, -9.127583699786111282, -10.13316557810918894 ) ) ;
#23154 = ORIENTED_EDGE ( 'NONE', *, *, #1932, .T. ) ;
#23155 = AXIS2_PLACEMENT_3D ( 'NONE', #347, #21071, #13257 ) ;
#23156 = CARTESIAN_POINT ( 'NONE',  ( 41.99999999999999289, 6.904644888889564703E-15, 10.50249999999999950 ) ) ;
#23157 = ORIENTED_EDGE ( 'NONE', *, *, #317, .F. ) ;
#23158 = EDGE_LOOP ( 'NONE', ( #23002, #6304, #11114, #14732 ) ) ;
#23159 = DIRECTION ( 'NONE',  ( 0.000000000000000000, 0.000000000000000000, 1.000000000000000000 ) ) ;
#23160 = CARTESIAN_POINT ( 'NONE',  ( -10.83999999999999986, -14.99147757894464306, 15.50000000000000000 ) ) ;
#23161 = EDGE_LOOP ( 'NONE', ( #13003, #1896, #6003, #10605 ) ) ;
#23162 = EDGE_CURVE ( 'NONE', #4642, #6224, #2168, .T. ) ;
#23163 = CARTESIAN_POINT ( 'NONE',  ( -42.00000000000000000, -6.000000000000000888, 12.00000000000000000 ) ) ;
#23164 = CARTESIAN_POINT ( 'NONE',  ( 83.30704456891035647, 7.562528597612068045E-15, 0.000000000000000000 ) ) ;
#23165 = EDGE_CURVE ( 'NONE', #21057, #3216, #1789, .T. ) ;
#23166 = DIRECTION ( 'NONE',  ( -1.000000000000000000, 2.600433232233976523E-16, -0.000000000000000000 ) ) ;
#23167 = CARTESIAN_POINT ( 'NONE',  ( 74.57977184163763695, -1.078520768856852078E-29, 5.000000000000007994 ) ) ;
#23168 = EDGE_LOOP ( 'NONE', ( #5710, #295, #15144, #22257 ) ) ;
#23169 = CIRCLE ( 'NONE', #3664, 9.725923461386809521 ) ;
#23170 = VECTOR ( 'NONE', #23598, 1000.000000000000000 ) ;
#23171 = CARTESIAN_POINT ( 'NONE',  ( 57.42022815836235594, -4.999999999999999112, 0.000000000000000000 ) ) ;
#23172 = CARTESIAN_POINT ( 'NONE',  ( -1.749335460929532182, -9.337549220493269075, 3.500000000000028866 ) ) ;
#23173 = AXIS2_PLACEMENT_3D ( 'NONE', #19397, #11930, #10210 ) ;
#23174 = CARTESIAN_POINT ( 'NONE',  ( -27.70933665152131198, 40.41277845351217479, 11.00000000000000000 ) ) ;
#23175 = DIRECTION ( 'NONE',  ( -0.000000000000000000, -0.000000000000000000, -1.000000000000000000 ) ) ;
#23176 = LINE ( 'NONE', #9718, #2435 ) ;
#23177 = CARTESIAN_POINT ( 'NONE',  ( 58.87477361290780919, 5.000000000000016875, 6.123233995736777129E-16 ) ) ;
#23178 = DIRECTION ( 'NONE',  ( 0.000000000000000000, -1.000000000000000000, 0.000000000000000000 ) ) ;
#23179 = ORIENTED_EDGE ( 'NONE', *, *, #21342, .T. ) ;
#23180 = CARTESIAN_POINT ( 'NONE',  ( 2.682529543900284974, -8.255977015246234174, -4.233165578109187699 ) ) ;
#23181 = ORIENTED_EDGE ( 'NONE', *, *, #1, .T. ) ;
#23182 = AXIS2_PLACEMENT_3D ( 'NONE', #23344, #14394, #20507 ) ;
#23183 = ORIENTED_EDGE ( 'NONE', *, *, #15201, .T. ) ;
#23184 = CARTESIAN_POINT ( 'NONE',  ( 2.935661446562616295, -9.035036904803758873, 7.659589141758144315 ) ) ;
#23185 = CARTESIAN_POINT ( 'NONE',  ( 5.871322893123449127, 8.081182679344781405, 11.50674201446023126 ) ) ;
#23186 = CIRCLE ( 'NONE', #12641, 11.00000000000001066 ) ;
#23187 = ORIENTED_EDGE ( 'NONE', *, *, #3296, .T. ) ;
#23188 = FACE_OUTER_BOUND ( 'NONE', #6600, .T. ) ;
#23189 = AXIS2_PLACEMENT_3D ( 'NONE', #21459, #1093, #4750 ) ;
#23190 = CARTESIAN_POINT ( 'NONE',  ( 37.00000000000000711, 29.50000000000000355, 12.00000000000000000 ) ) ;
#23191 = ADVANCED_FACE ( 'NONE', ( #2407 ), #14006, .F. ) ;
#23192 = CARTESIAN_POINT ( 'NONE',  ( 42.00000000000000000, -4.000000000000015099, 9.500000000000000000 ) ) ;
#23193 = DIRECTION ( 'NONE',  ( -1.000000000000000000, 0.000000000000000000, 0.000000000000000000 ) ) ;
#23194 = EDGE_CURVE ( 'NONE', #16878, #2131, #15404, .T. ) ;
#23195 = VECTOR ( 'NONE', #1085, 1000.000000000000000 ) ;
#23196 = CARTESIAN_POINT ( 'NONE',  ( -41.50000000000000000, -28.80990663662250739, 12.00000000000000000 ) ) ;
#23197 = DIRECTION ( 'NONE',  ( 0.000000000000000000, 0.000000000000000000, 1.000000000000000000 ) ) ;
#23198 = DIRECTION ( 'NONE',  ( -1.000000000000000000, -0.000000000000000000, -0.000000000000000000 ) ) ;
#23199 = DIRECTION ( 'NONE',  ( 0.000000000000000000, -0.000000000000000000, 1.000000000000000000 ) ) ;
#23200 = ORIENTED_EDGE ( 'NONE', *, *, #13630, .F. ) ;
#23201 = CARTESIAN_POINT ( 'NONE',  ( 75.45454545454545325, -4.172000000000000597, 5.616230220889771312E-16 ) ) ;
#23202 = VERTEX_POINT ( 'NONE', #958 ) ;
#23203 = DIRECTION ( 'NONE',  ( 0.000000000000000000, -1.000000000000000000, 0.000000000000000000 ) ) ;
#23204 = CARTESIAN_POINT ( 'NONE',  ( -5.618740543780279317, -7.334895587232010072, 12.29317507175855795 ) ) ;
#23206 = FACE_OUTER_BOUND ( 'NONE', #20347, .T. ) ;
#23205 = CIRCLE ( 'NONE', #22039, 0.4000000000000001887 ) ;
#23207 = CARTESIAN_POINT ( 'NONE',  ( 34.10000000000000853, 29.50000000000000000, 27.00000000000000000 ) ) ;
#23208 = CONICAL_SURFACE ( 'NONE', #8772, 5.000000000000007994, 0.9599310885968855844 ) ;
#23209 = CARTESIAN_POINT ( 'NONE',  ( 40.00000000000000000, 28.80990663662251450, 0.000000000000000000 ) ) ;
#23210 = ORIENTED_EDGE ( 'NONE', *, *, #15159, .T. ) ;
#23211 = TOROIDAL_SURFACE ( 'NONE', #1451, 11.23654394515110511, 0.9599481167642566204 ) ;
#23212 = DIRECTION ( 'NONE',  ( 0.5735764363510427177, -0.8191520442889941300, 1.003171929053527705E-16 ) ) ;
#23213 = CARTESIAN_POINT ( 'NONE',  ( -41.73082370883260239, 27.62204025492845361, -1.500000000000000000 ) ) ;
#23214 = VECTOR ( 'NONE', #21376, 1000.000000000000000 ) ;
#23215 = ORIENTED_EDGE ( 'NONE', *, *, #1640, .T. ) ;
#23216 = EDGE_CURVE ( 'NONE', #17583, #17352, #4928, .T. ) ;
#23217 = CARTESIAN_POINT ( 'NONE',  ( -7.685661446561619314, -5.583959896779019161, -6.406742014460233392 ) ) ;
#23218 = ORIENTED_EDGE ( 'NONE', *, *, #10513, .T. ) ;
#23219 = CARTESIAN_POINT ( 'NONE',  ( 0.000000000000000000, -15.03999999999999915, -27.00000000000000000 ) ) ;
#23220 = CARTESIAN_POINT ( 'NONE',  ( 5.365059087798939252, 7.384370330707087149, 8.933165578109187877 ) ) ;
#23221 = DIRECTION ( 'NONE',  ( -0.000000000000000000, -0.000000000000000000, 1.000000000000000000 ) ) ;
#23222 = CARTESIAN_POINT ( 'NONE',  ( 9.000000000000000000, 1.102182119232617714E-15, 15.00000000000000178 ) ) ;
#23223 = CARTESIAN_POINT ( 'NONE',  ( -14.51962751333974033, -3.765689428759031010, -8.721787840009202597 ) ) ;
#23224 = EDGE_CURVE ( 'NONE', #1494, #21150, #9948, .T. ) ;
#23225 = DIRECTION ( 'NONE',  ( -1.000000000000000000, 0.000000000000000000, 0.000000000000000000 ) ) ;
#23226 = ADVANCED_FACE ( 'NONE', ( #17797 ), #8384, .T. ) ;
#23227 = CONICAL_SURFACE ( 'NONE', #8003, 4.172000000000008590, 0.9599310885968742602 ) ;
#23228 = AXIS2_PLACEMENT_3D ( 'NONE', #20516, #19045, #18787 ) ;
#23229 = ORIENTED_EDGE ( 'NONE', *, *, #10244, .F. ) ;
#23230 = CONTEXT_DEPENDENT_SHAPE_REPRESENTATION ( #10087, #15501 ) ;
#23231 = ORIENTED_EDGE ( 'NONE', *, *, #834, .T. ) ;
#23232 = DIRECTION ( 'NONE',  ( -0.000000000000000000, -0.000000000000000000, -1.000000000000000000 ) ) ;
#23233 = AXIS2_PLACEMENT_3D ( 'NONE', #11757, #19232, #2515 ) ;
#23234 = CIRCLE ( 'NONE', #16966, 6.050000000006050982 ) ;
#23235 = CARTESIAN_POINT ( 'NONE',  ( -9.499999999999790390, -3.086737114213257804, -8.306742014460233747 ) ) ;
#23236 = ORIENTED_EDGE ( 'NONE', *, *, #24079, .F. ) ;
#23237 = ORIENTED_EDGE ( 'NONE', *, *, #4094, .F. ) ;
#23238 = CARTESIAN_POINT ( 'NONE',  ( -2.089646679935818430, -8.893998220852614267, -12.37209986270935502 ) ) ;
#23239 = CARTESIAN_POINT ( 'NONE',  ( 41.73082370883260239, 27.62204025492843940, -1.500000000000000000 ) ) ;
#23240 = ORIENTED_EDGE ( 'NONE', *, *, #11206, .T. ) ;
#23241 = DIRECTION ( 'NONE',  ( -1.000000000000000000, 0.000000000000000000, 0.000000000000000000 ) ) ;
#23242 = ORIENTED_EDGE ( 'NONE', *, *, #5193, .T. ) ;
#23243 = VECTOR ( 'NONE', #12506, 1000.000000000000227 ) ;
#23244 = CARTESIAN_POINT ( 'NONE',  ( 0.000000000000000000, 2.342598717236902939, -4.057500000000001883 ) ) ;
#23245 = CARTESIAN_POINT ( 'NONE',  ( 1.999999999999996669, 45.00000000000000000, -8.673617379884035472E-16 ) ) ;
#23246 = DIRECTION ( 'NONE',  ( -1.000000000000000000, -1.224606353822377258E-16, -0.000000000000000000 ) ) ;
#23247 = ADVANCED_FACE ( 'NONE', ( #19260 ), #2542, .F. ) ;
#23248 = CIRCLE ( 'NONE', #253, 5.025000000000002132 ) ;
#23249 = DIRECTION ( 'NONE',  ( -1.000000000000000000, 0.000000000000000000, 0.000000000000000000 ) ) ;
#23250 = VERTEX_POINT ( 'NONE', #17420 ) ;
#23251 = LINE ( 'NONE', #19206, #3286 ) ;
#23252 = FACE_OUTER_BOUND ( 'NONE', #5888, .T. ) ;
#23253 = FACE_OUTER_BOUND ( 'NONE', #15285, .T. ) ;
#23254 = ORIENTED_EDGE ( 'NONE', *, *, #10657, .T. ) ;
#23255 = VECTOR ( 'NONE', #12451, 1000.000000000000000 ) ;
#23256 = CARTESIAN_POINT ( 'NONE',  ( -7.685661446561619314, -5.583959896779019161, 5.259589141758143960 ) ) ;
#23257 = EDGE_LOOP ( 'NONE', ( #21651, #20423 ) ) ;
#23258 = EDGE_LOOP ( 'NONE', ( #16753, #23414, #7735, #19960, #22217, #10302, #2059, #10647 ) ) ;
#23259 = EDGE_CURVE ( 'NONE', #12845, #21315, #15453, .T. ) ;
#23260 = EDGE_CURVE ( 'NONE', #19153, #1596, #21808, .T. ) ;
#23261 = ORIENTED_EDGE ( 'NONE', *, *, #7581, .T. ) ;
#23262 = ORIENTED_EDGE ( 'NONE', *, *, #5824, .T. ) ;
#23263 = CARTESIAN_POINT ( 'NONE',  ( -1.374911245008260563, 8.680847955710920161, -3.184419859656034024 ) ) ;
#23264 = AXIS2_PLACEMENT_3D ( 'NONE', #2340, #15246, #9752 ) ;
#23265 = AXIS2_PLACEMENT_3D ( 'NONE', #14448, #10326, #18258 ) ;
#23266 = DIRECTION ( 'NONE',  ( -0.000000000000000000, -0.000000000000000000, -1.000000000000000000 ) ) ;
#23267 = FACE_OUTER_BOUND ( 'NONE', #20040, .T. ) ;
#23268 = AXIS2_PLACEMENT_3D ( 'NONE', #12604, #10650, #12249 ) ;
#23269 = EDGE_LOOP ( 'NONE', ( #6867, #6160, #6057, #23068 ) ) ;
#23270 = CYLINDRICAL_SURFACE ( 'NONE', #2501, 1.999999999999994449 ) ;
#23271 = FACE_OUTER_BOUND ( 'NONE', #314, .T. ) ;
#23272 = FACE_OUTER_BOUND ( 'NONE', #21120, .T. ) ;
#23273 = ORIENTED_EDGE ( 'NONE', *, *, #8251, .T. ) ;
#23274 = CARTESIAN_POINT ( 'NONE',  ( 80.39795365981946418, 7.562528597612068045E-15, 0.000000000000000000 ) ) ;
#23275 = CONICAL_SURFACE ( 'NONE', #12722, 8.500000000000000000, 0.9519047898634274141 ) ;
#23276 = CARTESIAN_POINT ( 'NONE',  ( -10.83999999999999986, -14.99147757894464306, 15.50000000000000000 ) ) ;
#23277 = DIRECTION ( 'NONE',  ( -1.000000000000000000, 0.000000000000000000, 0.000000000000000000 ) ) ;
#23278 = DIRECTION ( 'NONE',  ( 0.000000000000000000, 0.000000000000000000, 1.000000000000000000 ) ) ;
#23279 = LINE ( 'NONE', #19847, #15223 ) ;
#23280 = CARTESIAN_POINT ( 'NONE',  ( 61.78386452199871570, 7.420530141404717394E-15, 0.000000000000000000 ) ) ;
#23281 = CARTESIAN_POINT ( 'NONE',  ( 15.00000000000000355, 0.3238088414458227260, 9.499999999999989342 ) ) ;
#23282 = EDGE_CURVE ( 'NONE', #23301, #14197, #18156, .T. ) ;
#23283 = CARTESIAN_POINT ( 'NONE',  ( -5.365059087799948223, 7.384370330706355290, -5.333165578109190008 ) ) ;
#23284 = CIRCLE ( 'NONE', #4183, 4.250000000000000000 ) ;
#23285 = EDGE_LOOP ( 'NONE', ( #24052, #10834, #17014, #7946, #15055 ) ) ;
#23286 = ORIENTED_EDGE ( 'NONE', *, *, #12254, .T. ) ;
#23287 = ADVANCED_FACE ( 'NONE', ( #10455 ), #5089, .T. ) ;
#23288 = CARTESIAN_POINT ( 'NONE',  ( -5.365059087799947335, 7.384370330706355290, 9.333165578109190008 ) ) ;
#23289 = EDGE_CURVE ( 'NONE', #7597, #15489, #3383, .T. ) ;
#23290 = EDGE_LOOP ( 'NONE', ( #8573, #2077, #18536, #9894 ) ) ;
#23291 = DIRECTION ( 'NONE',  ( 1.000000000000000000, 0.000000000000000000, 0.000000000000000000 ) ) ;
#23292 = DIRECTION ( 'NONE',  ( -1.000000000000000000, -1.224606353822377258E-16, -0.000000000000000000 ) ) ;
#23293 = EDGE_LOOP ( 'NONE', ( #6377, #22507, #12044, #404, #15738, #6988, #6751, #17364, #4866, #24053, #7969, #17610, #7217, #21718, #8935, #735, #22983, #10321, #22198, #15318, #2142, #7400, #9171, #7944, #18721, #22208, #435, #11565, #13566, #7721, #3428, #8527, #6699, #20191, #3052, #6650, #6972, #17129, #12627, #19345, #7280, #22145, #12226, #22767, #2720, #8082, #14959, #21375 ) ) ;
#23294 = DIRECTION ( 'NONE',  ( 1.000000000000000000, 0.000000000000000000, 0.000000000000000000 ) ) ;
#23295 = CARTESIAN_POINT ( 'NONE',  ( 6.809999908187194197E-13, -9.988891130263535700, -11.55958914175814201 ) ) ;
#23296 = UNCERTAINTY_MEASURE_WITH_UNIT (LENGTH_MEASURE( 1.000000000000000082E-05 ), #19, 'distance_accuracy_value', 'NONE');
#23297 = CARTESIAN_POINT ( 'NONE',  ( -2.999999999999995559, 8.485281374238571317, 99.19969681971174680 ) ) ;
#23298 = DIRECTION ( 'NONE',  ( -0.000000000000000000, -0.000000000000000000, -1.000000000000000000 ) ) ;
#23299 = CARTESIAN_POINT ( 'NONE',  ( 9.500000000000000000, 1.163414459189985485E-15, 12.50000000000000000 ) ) ;
#23300 = VERTEX_POINT ( 'NONE', #3256 ) ;
#23301 = VERTEX_POINT ( 'NONE', #10801 ) ;
#23302 = LINE ( 'NONE', #21812, #20754 ) ;
#23303 = FACE_OUTER_BOUND ( 'NONE', #15142, .T. ) ;
#23304 = VERTEX_POINT ( 'NONE', #1454 ) ;
#23305 = CARTESIAN_POINT ( 'NONE',  ( 0.000000000000000000, 0.000000000000000000, -12.00000000000000000 ) ) ;
#23306 = ORIENTED_EDGE ( 'NONE', *, *, #17244, .T. ) ;
#23307 = DIRECTION ( 'NONE',  ( 1.000000000000000000, 0.000000000000000000, 0.000000000000000000 ) ) ;
#23308 = CARTESIAN_POINT ( 'NONE',  ( 85.05659179472598908, 7.420530141404717394E-15, 0.000000000000000000 ) ) ;
#23309 = DIRECTION ( 'NONE',  ( 4.613626265895764052E-16, -1.000000000000000000, 0.000000000000000000 ) ) ;
#23310 = EDGE_CURVE ( 'NONE', #23079, #702, #9190, .T. ) ;
#23311 = ORIENTED_EDGE ( 'NONE', *, *, #14008, .F. ) ;
#23312 = VECTOR ( 'NONE', #2839, 1000.000000000000000 ) ;
#23313 = ORIENTED_EDGE ( 'NONE', *, *, #13238, .F. ) ;
#23314 = ORIENTED_EDGE ( 'NONE', *, *, #22760, .T. ) ;
#23315 = CARTESIAN_POINT ( 'NONE',  ( -9.499999999999790390, -3.086737114213257804, 3.159589141758143871 ) ) ;
#23316 = CARTESIAN_POINT ( 'NONE',  ( -7.685661446561619314, -5.583959896779019161, 10.40674201446023339 ) ) ;
#23317 = AXIS2_PLACEMENT_3D ( 'NONE', #3614, #6930, #3495 ) ;
#23318 = ORIENTED_EDGE ( 'NONE', *, *, #17695, .T. ) ;
#23319 =( NAMED_UNIT ( * ) PLANE_ANGLE_UNIT ( ) SI_UNIT ( $, .RADIAN. ) );
#23320 = VECTOR ( 'NONE', #8071, 999.9999999999998863 ) ;
#23321 = DIRECTION ( 'NONE',  ( -0.7071067811865292541, 0.000000000000000000, -0.7071067811865658914 ) ) ;
#23322 = EDGE_CURVE ( 'NONE', #20548, #3419, #17913, .T. ) ;
#23323 = DIRECTION ( 'NONE',  ( 0.000000000000000000, -1.000000000000000000, 0.000000000000000000 ) ) ;
#23324 = DIRECTION ( 'NONE',  ( -0.000000000000000000, 1.000000000000000000, -0.000000000000000000 ) ) ;
#23325 = CARTESIAN_POINT ( 'NONE',  ( 23.90000000000000568, -29.50000000000000355, 0.000000000000000000 ) ) ;
#23326 = CARTESIAN_POINT ( 'NONE',  ( -10.49999999999999822, 1.285879139104720633E-15, -2.499999999999999556 ) ) ;
#23327 = DIRECTION ( 'NONE',  ( 0.000000000000000000, 0.000000000000000000, -1.000000000000000000 ) ) ;
#23328 = DIRECTION ( 'NONE',  ( -0.000000000000000000, -0.000000000000000000, -1.000000000000000000 ) ) ;
#23329 = FACE_OUTER_BOUND ( 'NONE', #10071, .T. ) ;
#23330 = EDGE_LOOP ( 'NONE', ( #4555, #16310 ) ) ;
#23331 = ORIENTED_EDGE ( 'NONE', *, *, #24070, .F. ) ;
#23332 = CARTESIAN_POINT ( 'NONE',  ( 0.9999999999999986677, 1.680940823232891723E-15, -13.72592346138681130 ) ) ;
#23333 = DIRECTION ( 'NONE',  ( 0.000000000000000000, -1.000000000000000000, 0.000000000000000000 ) ) ;
#23334 = AXIS2_PLACEMENT_3D ( 'NONE', #23764, #21925, #12642 ) ;
#23335 = CARTESIAN_POINT ( 'NONE',  ( 9.366788983124319401, -0.5939584231417279758, -12.13321101687572146 ) ) ;
#23336 = DIRECTION ( 'NONE',  ( 1.000000000000000000, 0.000000000000000000, 0.000000000000000000 ) ) ;
#23337 = AXIS2_PLACEMENT_3D ( 'NONE', #7792, #1122, #1238 ) ;
#23338 = DIRECTION ( 'NONE',  ( -1.000000000000000000, 0.000000000000000000, 0.000000000000000000 ) ) ;
#23339 = ADVANCED_FACE ( 'NONE', ( #12761 ), #3354, .T. ) ;
#23340 = EDGE_LOOP ( 'NONE', ( #18755, #6538, #5005, #8980 ) ) ;
#23341 = EDGE_CURVE ( 'NONE', #8229, #17123, #23647, .T. ) ;
#23342 = CARTESIAN_POINT ( 'NONE',  ( 69.63636363636364024, -4.172000000000000597, 5.616230220889771312E-16 ) ) ;
#23343 = ORIENTED_EDGE ( 'NONE', *, *, #18999, .T. ) ;
#23344 = CARTESIAN_POINT ( 'NONE',  ( -21.84999999999999787, -16.67999999999985050, 13.00000000000000178 ) ) ;
#23345 = VERTEX_POINT ( 'NONE', #12405 ) ;
#23346 = DIRECTION ( 'NONE',  ( 0.000000000000000000, 1.000000000000000000, -1.295896757998780388E-15 ) ) ;
#23347 = AXIS2_PLACEMENT_3D ( 'NONE', #13778, #13540, #23053 ) ;
#23348 = DIRECTION ( 'NONE',  ( 0.000000000000000000, -1.000000000000000000, 0.000000000000000000 ) ) ;
#23349 = CARTESIAN_POINT ( 'NONE',  ( -40.99749999999999517, 0.000000000000000000, 9.499999999999994671 ) ) ;
#23350 = DIRECTION ( 'NONE',  ( 0.000000000000000000, -1.000000000000000000, 0.000000000000000000 ) ) ;
#23351 = DIRECTION ( 'NONE',  ( -0.000000000000000000, 1.000000000000000000, -0.000000000000000000 ) ) ;
#23352 = VERTEX_POINT ( 'NONE', #5337 ) ;
#23353 = CARTESIAN_POINT ( 'NONE',  ( 35.99999999999992184, 59.99999999999998579, 12.50000000000000000 ) ) ;
#23354 = EDGE_CURVE ( 'NONE', #5912, #19325, #13090, .T. ) ;
#23355 = CARTESIAN_POINT ( 'NONE',  ( -7.685661446562381371, 5.583959896777970222, -10.85958914175814449 ) ) ;
#23356 = EDGE_LOOP ( 'NONE', ( #2196, #17010, #14022, #20126 ) ) ;
#23357 = ORIENTED_EDGE ( 'NONE', *, *, #22440, .T. ) ;
#23358 = DIRECTION ( 'NONE',  ( -1.000000000000000000, -1.224606353822377258E-16, -0.000000000000000000 ) ) ;
#23359 = FACE_BOUND ( 'NONE', #2285, .T. ) ;
#23360 = ORIENTED_EDGE ( 'NONE', *, *, #6908, .F. ) ;
#23361 = CARTESIAN_POINT ( 'NONE',  ( 67.60204634018053582, 6.123233995736675563E-16, -5.000000000000007994 ) ) ;
#23362 = EDGE_CURVE ( 'NONE', #10814, #9670, #8614, .T. ) ;
#23363 = EDGE_CURVE ( 'NONE', #12175, #13723, #5310, .T. ) ;
#23364 = ORIENTED_EDGE ( 'NONE', *, *, #4768, .F. ) ;
#23365 = DIRECTION ( 'NONE',  ( 0.000000000000000000, 0.000000000000000000, -1.000000000000000000 ) ) ;
#23366 = ADVANCED_FACE ( 'NONE', ( #21923 ), #1554, .F. ) ;
#23367 = CARTESIAN_POINT ( 'NONE',  ( 0.000000000000000000, 0.000000000000000000, 0.000000000000000000 ) ) ;
#23368 = EDGE_CURVE ( 'NONE', #6097, #7176, #20518, .T. ) ;
#23369 = SPHERICAL_SURFACE ( 'NONE', #2032, 1.500000000000000000 ) ;
#23370 = CYLINDRICAL_SURFACE ( 'NONE', #11014, 1.000000000000000888 ) ;
#23371 = FACE_OUTER_BOUND ( 'NONE', #23340, .T. ) ;
#23372 = ORIENTED_EDGE ( 'NONE', *, *, #10449, .F. ) ;
#23373 = CARTESIAN_POINT ( 'NONE',  ( 86.51113724927145654, 7.420530141404717394E-15, 0.000000000000000000 ) ) ;
#23374 = FACE_OUTER_BOUND ( 'NONE', #11210, .T. ) ;
#23375 = CARTESIAN_POINT ( 'NONE',  ( 63.81818181818181301, 7.491529369508391930E-15, 0.000000000000000000 ) ) ;
#23376 = CARTESIAN_POINT ( 'NONE',  ( 2.935661446562616295, -9.035036904803758873, 9.659589141758143427 ) ) ;
#23377 = AXIS2_PLACEMENT_3D ( 'NONE', #19059, #2333, #7562 ) ;
#23379 = ORIENTED_EDGE ( 'NONE', *, *, #677, .F. ) ;
#23378 = AXIS2_PLACEMENT_3D ( 'NONE', #19733, #5317, #14696 ) ;
#23380 = ORIENTED_EDGE ( 'NONE', *, *, #2757, .F. ) ;
#23381 = FACE_OUTER_BOUND ( 'NONE', #16745, .T. ) ;
#23382 = DIRECTION ( 'NONE',  ( 1.000000000000000000, 3.469446951953611033E-15, 0.000000000000000000 ) ) ;
#23383 = ADVANCED_FACE ( 'NONE', ( #23655 ), #21687, .T. ) ;
#23384 = DIRECTION ( 'NONE',  ( 0.4011779117250717785, 0.9160001545545232160, -0.000000000000000000 ) ) ;
#23385 = CARTESIAN_POINT ( 'NONE',  ( -41.00000000000000000, 6.000000000000000888, 11.00000000000000000 ) ) ;
#23386 = FACE_OUTER_BOUND ( 'NONE', #547, .T. ) ;
#23387 = EDGE_LOOP ( 'NONE', ( #4454, #15185, #1524, #6195 ) ) ;
#23388 = CARTESIAN_POINT ( 'NONE',  ( 1.686903467613876059E-18, 14.42592346043842255, 0.000000000000000000 ) ) ;
#23389 = DIRECTION ( 'NONE',  ( -0.5735764363510517105, -0.8191520442889879128, 0.000000000000000000 ) ) ;
#23390 = CARTESIAN_POINT ( 'NONE',  ( 9.500000000000209610, -3.086737114211962396, 5.106742014460234458 ) ) ;
#23391 = EDGE_CURVE ( 'NONE', #23753, #12216, #14236, .T. ) ;
#23392 = DIRECTION ( 'NONE',  ( -0.000000000000000000, -1.000000000000000000, -0.000000000000000000 ) ) ;
#23393 = EDGE_CURVE ( 'NONE', #8141, #21315, #19835, .T. ) ;
#23394 = CARTESIAN_POINT ( 'NONE',  ( 23.00000000000000000, 0.000000000000000000, 0.000000000000000000 ) ) ;
#23395 = CONICAL_SURFACE ( 'NONE', #20213, 1.024999999999999911, 0.7853981633974396193 ) ;
#23396 = CARTESIAN_POINT ( 'NONE',  ( 23.00000000000000000, 17.02535186363812514, -5.445458559198938175 ) ) ;
#23397 =( BOUNDED_CURVE ( )  B_SPLINE_CURVE ( 2, ( #18549, #12546, #5254, #14501, #21967, #12680, #20150, #9255, #18305, #20020, #9011 ),
 .UNSPECIFIED., .F., .T. ) 
 B_SPLINE_CURVE_WITH_KNOTS ( ( 3, 2, 2, 2, 2, 3 ),
 ( 0.006042316813506577906, 0.01999999999999999001, 0.03999999999999997308, 0.05999999999999994921, 0.07999999999999993228, 0.09999999999999992228 ),
 .UNSPECIFIED. ) 
 CURVE ( )  GEOMETRIC_REPRESENTATION_ITEM ( )  RATIONAL_B_SPLINE_CURVE ( ( 0.9793613297716632360, 0.9658431180202224908, 1.000000000000000000, 0.9510565162951535312, 1.000000000000000000, 0.9510565162951535312, 1.000000000000000000, 0.9510565162951535312, 1.000000000000000000, 0.9510565162951537532, 0.9999999999999997780 ) ) 
 REPRESENTATION_ITEM ( '' )  );
#23398 = CIRCLE ( 'NONE', #21451, 10.50249999999999950 ) ;
#23399 = DIRECTION ( 'NONE',  ( -0.7071067811865439090, 0.000000000000000000, -0.7071067811865512365 ) ) ;
#23400 = CARTESIAN_POINT ( 'NONE',  ( -7.022953521755574080, 5.102474405759713783, -7.433165578109188765 ) ) ;
#23401 = ORIENTED_EDGE ( 'NONE', *, *, #5751, .F. ) ;
#23402 = DIRECTION ( 'NONE',  ( -1.000000000000000000, -0.000000000000000000, -0.000000000000000000 ) ) ;
#23403 = VERTEX_POINT ( 'NONE', #19757 ) ;
#23404 = ORIENTED_EDGE ( 'NONE', *, *, #7213, .T. ) ;
#23405 =( NAMED_UNIT ( * ) PLANE_ANGLE_UNIT ( ) SI_UNIT ( $, .RADIAN. ) );
#23406 = DIRECTION ( 'NONE',  ( -0.000000000000000000, -0.000000000000000000, 1.000000000000000000 ) ) ;
#23407 = VERTEX_POINT ( 'NONE', #23997 ) ;
#23408 = EDGE_LOOP ( 'NONE', ( #23698, #20946, #22352, #12446, #16157 ) ) ;
#23409 = CARTESIAN_POINT ( 'NONE',  ( -9.499999999999790390, -3.086737114213257804, -5.159589141758141650 ) ) ;
#23410 = CIRCLE ( 'NONE', #9709, 18.50000000000000000 ) ;
#23411 = CARTESIAN_POINT ( 'NONE',  ( -0.9743949605962830551, 8.948941949199685553, 101.8440575432637587 ) ) ;
#23412 = FACE_OUTER_BOUND ( 'NONE', #10371, .T. ) ;
#23413 = FACE_OUTER_BOUND ( 'NONE', #11667, .T. ) ;
#23414 = ORIENTED_EDGE ( 'NONE', *, *, #12549, .T. ) ;
#23415 = DIRECTION ( 'NONE',  ( -0.000000000000000000, -0.000000000000000000, -1.000000000000000000 ) ) ;
#23416 = CARTESIAN_POINT ( 'NONE',  ( 23.00000000000000000, -15.26463740537718827, -9.300885435430258141 ) ) ;
#23417 = CARTESIAN_POINT ( 'NONE',  ( 9.500000000000000000, 6.470877716354879437E-13, -11.20674201446023410 ) ) ;
#23418 = VERTEX_POINT ( 'NONE', #12995 ) ;
#23419 = EDGE_CURVE ( 'NONE', #23514, #5942, #14939, .T. ) ;
#23420 = DIRECTION ( 'NONE',  ( -0.000000000000000000, -0.000000000000000000, -1.000000000000000000 ) ) ;
#23421 = LINE ( 'NONE', #12038, #1697 ) ;
#23422 = DIRECTION ( 'NONE',  ( 0.000000000000000000, -1.000000000000000000, 0.000000000000000000 ) ) ;
#23423 = ORIENTED_EDGE ( 'NONE', *, *, #23487, .F. ) ;
#23424 = CARTESIAN_POINT ( 'NONE',  ( -8.680847955710813579, -2.820578480814258437, -3.733165578109188587 ) ) ;
#23425 = EDGE_LOOP ( 'NONE', ( #19479, #11105, #15389, #21573 ) ) ;
#23426 = ORIENTED_EDGE ( 'NONE', *, *, #10812, .F. ) ;
#23427 = AXIS2_PLACEMENT_3D ( 'NONE', #10257, #19310, #13680 ) ;
#23428 = CARTESIAN_POINT ( 'NONE',  ( 7.685661446561619314, 5.583959896779020049, 4.259589141758143960 ) ) ;
#23429 = CARTESIAN_POINT ( 'NONE',  ( -9.500000000000211386, 3.086737114211961064, 10.10674201446023446 ) ) ;
#23430 = EDGE_LOOP ( 'NONE', ( #8339, #22868, #14986, #20224 ) ) ;
#23431 = DIRECTION ( 'NONE',  ( 0.9999999999999998890, 4.153214087920083129E-31, 5.886191147978195346E-17 ) ) ;
#23432 = FACE_OUTER_BOUND ( 'NONE', #2528, .T. ) ;
#23433 = DIRECTION ( 'NONE',  ( 0.000000000000000000, 0.000000000000000000, -1.000000000000000000 ) ) ;
#23434 = CARTESIAN_POINT ( 'NONE',  ( -9.000000000000000000, 0.000000000000000000, 0.9999999999999940048 ) ) ;
#23435 = ADVANCED_FACE ( 'NONE', ( #1906 ), #5701, .F. ) ;
#23436 = DIRECTION ( 'NONE',  ( -1.000000000000000000, 0.000000000000000000, 0.000000000000000000 ) ) ;
#23437 = DIRECTION ( 'NONE',  ( 0.9160001545545232160, -0.4011779117250717785, -0.000000000000000000 ) ) ;
#23438 = EDGE_CURVE ( 'NONE', #19878, #22118, #1422, .T. ) ;
#23440 = EDGE_CURVE ( 'NONE', #17472, #8169, #5806, .T. ) ;
#23439 = DIRECTION ( 'NONE',  ( 0.000000000000000000, 0.000000000000000000, 1.000000000000000000 ) ) ;
#23441 = EDGE_LOOP ( 'NONE', ( #15642, #20254, #6859, #1561 ) ) ;
#23442 = CONICAL_SURFACE ( 'NONE', #3547, 5.000000000000007994, 0.9599310885968855844 ) ;
#23443 = CARTESIAN_POINT ( 'NONE',  ( 41.00000000000000000, -4.000000000000015099, 8.500000000000000000 ) ) ;
#23444 = ORIENTED_EDGE ( 'NONE', *, *, #21474, .T. ) ;
#23445 = CYLINDRICAL_SURFACE ( 'NONE', #4339, 1.000000000000000888 ) ;
#23446 = CARTESIAN_POINT ( 'NONE',  ( 2.935661446561383503, 9.035036904804158553, 10.45958914175814414 ) ) ;
#23447 = CARTESIAN_POINT ( 'NONE',  ( -9.500000000000000000, -6.482511860946779655E-13, -10.20674201446023233 ) ) ;
#23448 = CARTESIAN_POINT ( 'NONE',  ( 41.00000000000000000, 4.999999999999986677, 11.00000000000000000 ) ) ;
#23449 = DIRECTION ( 'NONE',  ( -1.000000000000000000, -0.000000000000000000, 0.000000000000000000 ) ) ;
#23450 = ORIENTED_EDGE ( 'NONE', *, *, #7536, .F. ) ;
#23451 = ORIENTED_EDGE ( 'NONE', *, *, #17350, .T. ) ;
#23452 = CARTESIAN_POINT ( 'NONE',  ( 9.500000000000000000, 6.470877716354879437E-13, 4.059589141758143782 ) ) ;
#23453 = ORIENTED_EDGE ( 'NONE', *, *, #10125, .T. ) ;
#23454 = DIRECTION ( 'NONE',  ( -1.000000000000000000, 0.000000000000000000, 0.000000000000000000 ) ) ;
#23455 = CARTESIAN_POINT ( 'NONE',  ( -31.74999999999995737, 0.000000000000000000, 5.000000000000000888 ) ) ;
#23456 = SHAPE_REPRESENTATION ( 'Nipple', ( #8005 ), #10756 ) ;
#23457 = CARTESIAN_POINT ( 'NONE',  ( -20.85000000000000853, 15.04000000000000092, 25.00000000000000000 ) ) ;
#23458 = CIRCLE ( 'NONE', #3563, 9.000000000000001776 ) ;
#23459 = CARTESIAN_POINT ( 'NONE',  ( -31.74999999999995737, 0.000000000000000000, 0.000000000000000000 ) ) ;
#23460 = VERTEX_POINT ( 'NONE', #7618 ) ;
#23461 = EDGE_CURVE ( 'NONE', #11156, #15083, #1794, .T. ) ;
#23462 = LINE ( 'NONE', #8554, #23627 ) ;
#23463 = ADVANCED_FACE ( 'NONE', ( #11522 ), #22769, .F. ) ;
#23464 = VERTEX_POINT ( 'NONE', #14819 ) ;
#23465 = EDGE_LOOP ( 'NONE', ( #5331, #429 ) ) ;
#23466 = LINE ( 'NONE', #16135, #23170 ) ;
#23467 = ORIENTED_EDGE ( 'NONE', *, *, #22125, .T. ) ;
#23468 = VECTOR ( 'NONE', #23175, 1000.000000000000000 ) ;
#23469 = VECTOR ( 'NONE', #21132, 1000.000000000000000 ) ;
#23470 = AXIS2_PLACEMENT_3D ( 'NONE', #2693, #8156, #23065 ) ;
#23471 = ORIENTED_EDGE ( 'NONE', *, *, #1753, .F. ) ;
#23472 = CARTESIAN_POINT ( 'NONE',  ( -9.999999999999998224, 0.000000000000000000, 15.50000000000000000 ) ) ;
#23473 = DIRECTION ( 'NONE',  ( -1.000000000000000000, -1.224606353822377258E-16, -0.000000000000000000 ) ) ;
#23474 = DIRECTION ( 'NONE',  ( 1.000000000000000000, 0.000000000000000000, 0.000000000000000000 ) ) ;
#23475 = AXIS2_PLACEMENT_3D ( 'NONE', #15733, #1113, #856 ) ;
#23476 = CARTESIAN_POINT ( 'NONE',  ( 6.250000000000000000, 10.82531754730548279, -2.500000000000000000 ) ) ;
#23477 = CARTESIAN_POINT ( 'NONE',  ( 0.000000000000000000, 0.000000000000000000, 0.000000000000000000 ) ) ;
#23478 = ORIENTED_EDGE ( 'NONE', *, *, #14811, .F. ) ;
#23479 = DIRECTION ( 'NONE',  ( -0.000000000000000000, 0.000000000000000000, 1.000000000000000000 ) ) ;
#23480 = DIRECTION ( 'NONE',  ( 1.000000000000000000, 0.000000000000000000, 0.000000000000000000 ) ) ;
#23481 = DIRECTION ( 'NONE',  ( 0.000000000000000000, 0.000000000000000000, 1.000000000000000000 ) ) ;
#23482 = CARTESIAN_POINT ( 'NONE',  ( -7.685661446562381371, 5.583959896777970222, 8.859589141758144493 ) ) ;
#23483 = EDGE_CURVE ( 'NONE', #21197, #19750, #3742, .T. ) ;
#23484 = ADVANCED_FACE ( 'NONE', ( #20822 ), #2266, .T. ) ;
#23485 = ORIENTED_EDGE ( 'NONE', *, *, #8619, .T. ) ;
#23486 = VERTEX_POINT ( 'NONE', #11261 ) ;
#23487 = EDGE_CURVE ( 'NONE', #8991, #6915, #12697, .T. ) ;
#23488 = EDGE_LOOP ( 'NONE', ( #1042, #23966, #5800, #22804 ) ) ;
#23489 = AXIS2_PLACEMENT_3D ( 'NONE', #20647, #6007, #9754 ) ;
#23491 = VECTOR ( 'NONE', #17539, 1000.000000000000000 ) ;
#23490 = DIRECTION ( 'NONE',  ( -0.000000000000000000, -0.000000000000000000, -1.000000000000000000 ) ) ;
#23492 = EDGE_CURVE ( 'NONE', #1372, #18218, #9686, .T. ) ;
#23493 = CIRCLE ( 'NONE', #19614, 5.000000000000007994 ) ;
#23494 = AXIS2_PLACEMENT_3D ( 'NONE', #9043, #13068, #18690 ) ;
#23495 = CARTESIAN_POINT ( 'NONE',  ( 40.00000000000000711, 29.50000000000000000, 27.00000000000000000 ) ) ;
#23496 = CARTESIAN_POINT ( 'NONE',  ( 68.18181818181818699, 4.172000000000015696, 0.000000000000000000 ) ) ;
#23497 = CARTESIAN_POINT ( 'NONE',  ( -17.32314925601269806, -8.733074366907757735, -3.769949228126193486 ) ) ;
#23498 = AXIS2_PLACEMENT_3D ( 'NONE', #5875, #2098, #18695 ) ;
#23499 = DIRECTION ( 'NONE',  ( 1.000000000000000000, -4.613626265895763066E-16, 0.000000000000000000 ) ) ;
#23500 = ORIENTED_EDGE ( 'NONE', *, *, #20841, .T. ) ;
#23501 = DIRECTION ( 'NONE',  ( 0.000000000000000000, 0.000000000000000000, 1.000000000000000000 ) ) ;
#23502 = DIRECTION ( 'NONE',  ( 1.000000000000000000, 0.000000000000000000, -0.000000000000000000 ) ) ;
#23503 = FACE_OUTER_BOUND ( 'NONE', #22607, .T. ) ;
#23504 = CARTESIAN_POINT ( 'NONE',  ( -31.10231664966676846, -45.36128193761570770, 11.00000000000000000 ) ) ;
#23505 = CARTESIAN_POINT ( 'NONE',  ( 17.52854577772373190, -9.313395544511447355, -1.935253206038896279 ) ) ;
#23506 = CIRCLE ( 'NONE', #15699, 5.000000000000007994 ) ;
#23507 = CARTESIAN_POINT ( 'NONE',  ( 9.500000000000000000, 1.163414459189985485E-15, -12.00000000000000000 ) ) ;
#23508 = CARTESIAN_POINT ( 'NONE',  ( -8.680847955711007202, -5.923547351154968927E-13, -3.633165578109188054 ) ) ;
#23509 = AXIS2_PLACEMENT_3D ( 'NONE', #22107, #10486, #9135 ) ;
#23510 = AXIS2_PLACEMENT_3D ( 'NONE', #18007, #18361, #1649 ) ;
#23511 = ORIENTED_EDGE ( 'NONE', *, *, #16180, .F. ) ;
#23512 = CARTESIAN_POINT ( 'NONE',  ( 0.000000000000000000, 0.000000000000000000, 15.50000000000000000 ) ) ;
#23513 = EDGE_CURVE ( 'NONE', #4806, #5924, #3609, .T. ) ;
#23514 = VERTEX_POINT ( 'NONE', #9220 ) ;
#23515 = VECTOR ( 'NONE', #2066, 1000.000000000000000 ) ;
#23516 = CARTESIAN_POINT ( 'NONE',  ( -5.365059087798939252, -7.384370330707086261, 5.933165578109187877 ) ) ;
#23517 = AXIS2_PLACEMENT_3D ( 'NONE', #3644, #7405, #14847 ) ;
#23518 = APPLICATION_PROTOCOL_DEFINITION ( 'draft international standard', 'automotive_design', 1998, #10238 ) ;
#23519 = LINE ( 'NONE', #21689, #22215 ) ;
#23520 = ORIENTED_EDGE ( 'NONE', *, *, #10686, .F. ) ;
#23521 = ORIENTED_EDGE ( 'NONE', *, *, #1725, .T. ) ;
#23522 = ADVANCED_FACE ( 'NONE', ( #4106 ), #17013, .F. ) ;
#23523 = CARTESIAN_POINT ( 'NONE',  ( -41.49999999999999289, 27.79189783386526358, 27.00000000000000000 ) ) ;
#23524 = CARTESIAN_POINT ( 'NONE',  ( 5.871322893123449127, 8.081182679344781405, -6.359589141758142716 ) ) ;
#23525 = ADVANCED_FACE ( 'NONE', ( #22639 ), #5562, .T. ) ;
#23526 = LINE ( 'NONE', #19756, #5604 ) ;
#23528 = AXIS2_PLACEMENT_3D ( 'NONE', #10375, #4909, #19794 ) ;
#23527 = DIRECTION ( 'NONE',  ( -0.8660254037844387076, 0.4999999999999999445, 0.000000000000000000 ) ) ;
#23529 = CYLINDRICAL_SURFACE ( 'NONE', #7583, 5.100000000000000533 ) ;
#23530 = VERTEX_POINT ( 'NONE', #9571 ) ;
#23531 = AXIS2_PLACEMENT_3D ( 'NONE', #15273, #6263, #23113 ) ;
#23532 = DIRECTION ( 'NONE',  ( -1.000000000000000000, 0.000000000000000000, 0.000000000000000000 ) ) ;
#23533 = AXIS2_PLACEMENT_3D ( 'NONE', #15662, #19720, #23133 ) ;
#23534 = CIRCLE ( 'NONE', #16863, 9.725923461386811297 ) ;
#23535 = VECTOR ( 'NONE', #1892, 1000.000000000000000 ) ;
#23536 = FACE_OUTER_BOUND ( 'NONE', #3749, .T. ) ;
#23537 = DIRECTION ( 'NONE',  ( 0.000000000000000000, 0.000000000000000000, 1.000000000000000000 ) ) ;
#23538 = CARTESIAN_POINT ( 'NONE',  ( -34.10000000000000142, 29.49999999999999645, 12.00000000000000000 ) ) ;
#23539 = AXIS2_PLACEMENT_3D ( 'NONE', #18265, #11150, #9322 ) ;
#23540 = CARTESIAN_POINT ( 'NONE',  ( 5.000000000000000000, 4.685197434473818312, -1.301042606982605321E-15 ) ) ;
#23541 = CARTESIAN_POINT ( 'NONE',  ( -9.999999999999998224, 0.000000000000000000, 0.000000000000000000 ) ) ;
#23542 = EDGE_LOOP ( 'NONE', ( #261, #12307 ) ) ;
#23543 = ORIENTED_EDGE ( 'NONE', *, *, #11448, .F. ) ;
#23544 = ORIENTED_EDGE ( 'NONE', *, *, #13290, .T. ) ;
#23545 = CARTESIAN_POINT ( 'NONE',  ( 5.871322893123449127, 8.081182679344781405, 4.359589141758143604 ) ) ;
#23546 = CARTESIAN_POINT ( 'NONE',  ( 9.499999999999790390, 3.086737114213260025, 7.306742014460234635 ) ) ;
#23547 = DIRECTION ( 'NONE',  ( 1.000000000000000000, 1.224606353822377258E-16, 0.000000000000000000 ) ) ;
#23548 = AXIS2_PLACEMENT_3D ( 'NONE', #6000, #11219, #1962 ) ;
#23549 = ORIENTED_EDGE ( 'NONE', *, *, #16550, .F. ) ;
#23550 = DIRECTION ( 'NONE',  ( 1.110223024625157033E-16, -1.000000000000000222, -6.514579901954854577E-17 ) ) ;
#23551 = AXIS2_PLACEMENT_3D ( 'NONE', #3183, #18087, #1601 ) ;
#23552 = DIRECTION ( 'NONE',  ( 0.000000000000000000, 0.000000000000000000, 1.000000000000000000 ) ) ;
#23553 = VECTOR ( 'NONE', #16265, 1000.000000000000000 ) ;
#23554 = DIRECTION ( 'NONE',  ( 1.000000000000000000, -2.600433232233976523E-16, 0.000000000000000000 ) ) ;
#23555 = CARTESIAN_POINT ( 'NONE',  ( 87.09090909090909349, 7.491529369508391930E-15, 0.000000000000000000 ) ) ;
#23556 = EDGE_CURVE ( 'NONE', #20733, #4776, #18570, .T. ) ;
#23557 = AXIS2_PLACEMENT_3D ( 'NONE', #22923, #13632, #4136 ) ;
#23558 = ADVANCED_FACE ( 'NONE', ( #17022 ), #13359, .T. ) ;
#23559 = VECTOR ( 'NONE', #18522, 1000.000000000000000 ) ;
#23560 = DIRECTION ( 'NONE',  ( -1.000000000000000000, 0.000000000000000000, 0.000000000000000000 ) ) ;
#23561 = CARTESIAN_POINT ( 'NONE',  ( -12.50000000000000178, 1.672973214995343413E-15, -2.500000000000000000 ) ) ;
#23562 = LINE ( 'NONE', #16226, #1642 ) ;
#23563 = VERTEX_POINT ( 'NONE', #85 ) ;
#23564 = CARTESIAN_POINT ( 'NONE',  ( 35.99999999999999289, -51.00000000000000711, 12.50000000000000000 ) ) ;
#23565 = VERTEX_POINT ( 'NONE', #2749 ) ;
#23566 = CARTESIAN_POINT ( 'NONE',  ( 85.63636363636365445, 7.491529369508391930E-15, 0.000000000000000000 ) ) ;
#23567 = DIRECTION ( 'NONE',  ( 0.000000000000000000, 0.000000000000000000, -1.000000000000000000 ) ) ;
#23568 = CARTESIAN_POINT ( 'NONE',  ( -7.725160277709925083, 5.537733574950152615, -3.500137086806215603 ) ) ;
#23569 = DIRECTION ( 'NONE',  ( -1.000000000000000000, 0.000000000000000000, 0.000000000000000000 ) ) ;
#23570 = CIRCLE ( 'NONE', #21991, 8.000000000000000000 ) ;
#23571 = VECTOR ( 'NONE', #21858, 1000.000000000000000 ) ;
#23572 = CARTESIAN_POINT ( 'NONE',  ( 71.67068093254673045, -1.078520768856852078E-29, 5.000000000000007994 ) ) ;
#23573 = EDGE_LOOP ( 'NONE', ( #18121, #13411, #14893, #12792, #16493 ) ) ;
#23574 = ADVANCED_FACE ( 'NONE', ( #13494 ), #4939, .F. ) ;
#23575 = CIRCLE ( 'NONE', #964, 6.050000000006051870 ) ;
#23576 = DIRECTION ( 'NONE',  ( 0.000000000000000000, 0.000000000000000000, 1.000000000000000000 ) ) ;
#23577 = ORIENTED_EDGE ( 'NONE', *, *, #2740, .F. ) ;
#23578 = CARTESIAN_POINT ( 'NONE',  ( 0.000000000000000000, 0.000000000000000000, 4.000000000000000000 ) ) ;
#23579 = CIRCLE ( 'NONE', #13026, 20.85000000000000497 ) ;
#23580 = ORIENTED_EDGE ( 'NONE', *, *, #22475, .F. ) ;
#23581 = EDGE_CURVE ( 'NONE', #9768, #14927, #20944, .T. ) ;
#23582 = CARTESIAN_POINT ( 'NONE',  ( -5.622572944242077574E-13, 8.680847955711007202, 3.133165578109187610 ) ) ;
#23583 = DIRECTION ( 'NONE',  ( -0.000000000000000000, -0.000000000000000000, -1.000000000000000000 ) ) ;
#23584 = ORIENTED_EDGE ( 'NONE', *, *, #11836, .F. ) ;
#23585 = LINE ( 'NONE', #23703, #282 ) ;
#23586 = CIRCLE ( 'NONE', #14602, 4.172000000000008590 ) ;
#23587 = DIRECTION ( 'NONE',  ( 1.000000000000000000, 0.000000000000000000, 0.000000000000000000 ) ) ;
#23588 = EDGE_CURVE ( 'NONE', #13080, #15663, #12001, .T. ) ;
#23589 = DIRECTION ( 'NONE',  ( 0.000000000000000000, -1.000000000000000000, 0.000000000000000000 ) ) ;
#23590 = CIRCLE ( 'NONE', #16168, 6.050000000006052758 ) ;
#23591 = VECTOR ( 'NONE', #7715, 1000.000000000000000 ) ;
#23592 = CYLINDRICAL_SURFACE ( 'NONE', #5294, 1.500000000000001332 ) ;
#23593 = AXIS2_PLACEMENT_3D ( 'NONE', #6201, #13637, #19133 ) ;
#23594 = CARTESIAN_POINT ( 'NONE',  ( -2.935661446561384391, -9.035036904804158553, -4.606742014460233570 ) ) ;
#23595 = EDGE_LOOP ( 'NONE', ( #15599, #20995 ) ) ;
#23596 = AXIS2_PLACEMENT_3D ( 'NONE', #564, #15297, #11754 ) ;
#23597 = ORIENTED_EDGE ( 'NONE', *, *, #4094, .T. ) ;
#23598 = DIRECTION ( 'NONE',  ( 1.000000000000000000, 0.000000000000000000, 0.000000000000000000 ) ) ;
#23599 = DIRECTION ( 'NONE',  ( 0.7071067811865660024, 8.659560562355159656E-17, -0.7071067811865291430 ) ) ;
#23600 = VECTOR ( 'NONE', #17061, 999.9999999999998863 ) ;
#23601 = AXIS2_PLACEMENT_3D ( 'NONE', #2778, #2543, #11660 ) ;
#23602 = ORIENTED_EDGE ( 'NONE', *, *, #21191, .T. ) ;
#23603 = EDGE_CURVE ( 'NONE', #5195, #14197, #4225, .T. ) ;
#23604 = DIRECTION ( 'NONE',  ( 0.000000000000000000, -1.000000000000000000, 0.000000000000000000 ) ) ;
#23605 = DIRECTION ( 'NONE',  ( -1.000000000000000000, 0.000000000000000000, 0.000000000000000000 ) ) ;
#23606 =( BOUNDED_SURFACE ( )  B_SPLINE_SURFACE ( 1, 2, ( 
 ( #12024, #15568, #21449, #1086, #12147, #23295, #10330, #19497, #21203, #19256, #2774, #6305, #15323, #6078, #20964, #2405, #4249, #589, #8008, #17418, #22922, #13753, #13629, #10556, #8963, #1551, #19974, #10451, #23758, #1317, #3134, #6806, #20220, #18021, #22056, #5203, #5333, #3491, #17911, #10681, #14345, #4868, #1197, #1450, #23652, #21806, #18152, #10904, #12503, #3032, #21576, #14232, #5087, #18374, #23868, #8860, #3254, #23524, #12280, #8741, #16193, #12757, #21694, #3379, #8505, #16299, #7028, #19753, #15947, #23409, #14585, #7149, #4987, #6683, #6924, #8611, #14115, #12635, #16060, #14456, #12400, #21921, #20103, #19862, #10798, #18263, #16411, #18622, #22173, #14935, #5915, #9433, #5802, #13354, #22410, #20446, #15164 ),
 ( #22280, #18730, #16541, #3737, #9565, #20816, #206, #9094, #18859, #13118, #5447, #13228, #12866, #16891, #2140, #23992, #22634, #17017, #7610, #7732, #1788, #322, #4102, #11258, #16664, #2008, #12991, #16763, #7274, #14712, #11516, #5693, #11148, #5558, #1903, #3606, #20575, #20325, #9217, #1669, #9319, #11028, #80, #7485, #18502, #11381, #20536, #7378, #14815, #3852, #15059, #22528, #20682, #3965, #13601, #6164, #17132, #19355, #15537, #11745, #21046, #23004, #19101, #11996, #2374, #17614, #2262, #7979, #2507, #21169, #4473, #4595, #19224, #21302, #13718, #686, #8348, #19467, #17389, #2631, #11630, #4220, #4336, #2744, #10159, #20940, #9928, #21417, #8093, #923, #6275, #558, #15426, #9791, #11884, #23263, #22765 ) ),
 .UNSPECIFIED., .F., .F., .T. ) 
 B_SPLINE_SURFACE_WITH_KNOTS ( ( 2, 2 ),
 ( 3, 2, 2, 2, 2, 2, 2, 2, 2, 2, 2, 2, 2, 2, 2, 2, 2, 2, 2, 2, 2, 2, 2, 2, 2, 2, 2, 2, 2, 2, 2, 2, 2, 2, 2, 2, 2, 2, 2, 2, 2, 2, 2, 2, 2, 2, 2, 2, 3 ),
 ( 0.000000000000000000, 1.000000000000000000 ),
 ( 0.000000000000000000, 0.02000000000000000042, 0.04000000000000000083, 0.05999999999999999778, 0.08000000000000000167, 0.1000000000000000056, 0.1199999999999999956, 0.1400000000000000133, 0.1600000000000000033, 0.1799999999999999933, 0.2000000000000000111, 0.2200000000000000011, 0.2399999999999999911, 0.2600000000000000089, 0.2800000000000000266, 0.2999999999999999889, 0.3200000000000000067, 0.3400000000000000244, 0.3599999999999999867, 0.3800000000000000044, 0.4000000000000000222, 0.4199999999999999845, 0.4400000000000000022, 0.4600000000000000200, 0.4799999999999999822, 0.5000000000000000000, 0.5200000000000000178, 0.5400000000000000355, 0.5600000000000000533, 0.5799999999999999600, 0.5999999999999999778, 0.6199999999999999956, 0.6400000000000000133, 0.6600000000000000311, 0.6800000000000000488, 0.6999999999999999556, 0.7199999999999999734, 0.7399999999999999911, 0.7600000000000000089, 0.7800000000000000266, 0.8000000000000000444, 0.8199999999999999512, 0.8399999999999999689, 0.8599999999999999867, 0.8800000000000000044, 0.9000000000000000222, 0.9200000000000000400, 0.9399999999999999467, 0.9500000000000000666 ),
 .UNSPECIFIED. ) 
 GEOMETRIC_REPRESENTATION_ITEM ( )  RATIONAL_B_SPLINE_SURFACE ( (
 ( 1.000000000000000000, 0.9510565162951535312, 1.000000000000000000, 0.9510565162951535312, 1.000000000000000000, 0.9510565162951535312, 1.000000000000000000, 0.9510565162951535312, 1.000000000000000000, 0.9510565162951535312, 1.000000000000000000, 0.9510565162951535312, 1.000000000000000000, 0.9510565162951535312, 1.000000000000000000, 0.9510565162951535312, 1.000000000000000000, 0.9510565162951535312, 1.000000000000000000, 0.9510565162951535312, 1.000000000000000000, 0.9510565162951535312, 1.000000000000000000, 0.9510565162951535312, 1.000000000000000000, 0.9510565162951535312, 1.000000000000000000, 0.9510565162951535312, 1.000000000000000000, 0.9510565162951535312, 1.000000000000000000, 0.9510565162951535312, 1.000000000000000000, 0.9510565162951535312, 1.000000000000000000, 0.9510565162951535312, 1.000000000000000000, 0.9510565162951535312, 1.000000000000000000, 0.9510565162951535312, 1.000000000000000000, 0.9510565162951535312, 1.000000000000000000, 0.9510565162951535312, 1.000000000000000000, 0.9510565162951535312, 1.000000000000000000, 0.9510565162951535312, 1.000000000000000000, 0.9510565162951535312, 1.000000000000000000, 0.9510565162951535312, 1.000000000000000000, 0.9510565162951535312, 1.000000000000000000, 0.9510565162951535312, 1.000000000000000000, 0.9510565162951535312, 1.000000000000000000, 0.9510565162951535312, 1.000000000000000000, 0.9510565162951535312, 1.000000000000000000, 0.9510565162951535312, 1.000000000000000000, 0.9510565162951535312, 1.000000000000000000, 0.9510565162951535312, 1.000000000000000000, 0.9510565162951535312, 1.000000000000000000, 0.9510565162951535312, 1.000000000000000000, 0.9510565162951535312, 1.000000000000000000, 0.9510565162951535312, 1.000000000000000000, 0.9510565162951535312, 1.000000000000000000, 0.9510565162951535312, 1.000000000000000000, 0.9510565162951535312, 1.000000000000000000, 0.9510565162951535312, 1.000000000000000000, 0.9510565162951535312, 1.000000000000000000, 0.9510565162951535312, 1.000000000000000000, 0.9510565162951535312, 1.000000000000000000, 0.9510565162951535312, 1.000000000000000000, 0.9510565162951535312, 1.000000000000000000, 0.9755282581475764880, 0.9755282581475768211),
 ( 1.000000000000000000, 0.9510565162951535312, 1.000000000000000000, 0.9510565162951535312, 1.000000000000000000, 0.9510565162951535312, 1.000000000000000000, 0.9510565162951535312, 1.000000000000000000, 0.9510565162951535312, 1.000000000000000000, 0.9510565162951535312, 1.000000000000000000, 0.9510565162951535312, 1.000000000000000000, 0.9510565162951535312, 1.000000000000000000, 0.9510565162951535312, 1.000000000000000000, 0.9510565162951535312, 1.000000000000000000, 0.9510565162951535312, 1.000000000000000000, 0.9510565162951535312, 1.000000000000000000, 0.9510565162951535312, 1.000000000000000000, 0.9510565162951535312, 1.000000000000000000, 0.9510565162951535312, 1.000000000000000000, 0.9510565162951535312, 1.000000000000000000, 0.9510565162951535312, 1.000000000000000000, 0.9510565162951535312, 1.000000000000000000, 0.9510565162951535312, 1.000000000000000000, 0.9510565162951535312, 1.000000000000000000, 0.9510565162951535312, 1.000000000000000000, 0.9510565162951535312, 1.000000000000000000, 0.9510565162951535312, 1.000000000000000000, 0.9510565162951535312, 1.000000000000000000, 0.9510565162951535312, 1.000000000000000000, 0.9510565162951535312, 1.000000000000000000, 0.9510565162951535312, 1.000000000000000000, 0.9510565162951535312, 1.000000000000000000, 0.9510565162951535312, 1.000000000000000000, 0.9510565162951535312, 1.000000000000000000, 0.9510565162951535312, 1.000000000000000000, 0.9510565162951535312, 1.000000000000000000, 0.9510565162951535312, 1.000000000000000000, 0.9510565162951535312, 1.000000000000000000, 0.9510565162951535312, 1.000000000000000000, 0.9510565162951535312, 1.000000000000000000, 0.9510565162951535312, 1.000000000000000000, 0.9510565162951535312, 1.000000000000000000, 0.9510565162951535312, 1.000000000000000000, 0.9510565162951535312, 1.000000000000000000, 0.9510565162951535312, 1.000000000000000000, 0.9510565162951535312, 1.000000000000000000, 0.9510565162951535312, 1.000000000000000000, 0.9510565162951535312, 1.000000000000000000, 0.9510565162951535312, 1.000000000000000000, 0.9510565162951535312, 1.000000000000000000, 0.9510565162951535312, 1.000000000000000000, 0.9755282581475764880, 0.9755282581475768211) ) ) 
 REPRESENTATION_ITEM ( '' )  SURFACE ( )  );
#23607 = LINE ( 'NONE', #3209, #5980 ) ;
#23608 = ORIENTED_EDGE ( 'NONE', *, *, #13642, .F. ) ;
#23609 = DIRECTION ( 'NONE',  ( 1.000000000000000000, 0.000000000000000000, 0.000000000000000000 ) ) ;
#23610 = ADVANCED_FACE ( 'NONE', ( #23271 ), #7983, .F. ) ;
#23611 = DIRECTION ( 'NONE',  ( 0.000000000000000000, -0.000000000000000000, 1.000000000000000000 ) ) ;
#23612 = CARTESIAN_POINT ( 'NONE',  ( 9.500000000000000000, 6.470877716354879437E-13, -7.206742014460234103 ) ) ;
#23613 = CIRCLE ( 'NONE', #7270, 8.000000000000021316 ) ;
#23614 = DIRECTION ( 'NONE',  ( -0.000000000000000000, -0.000000000000000000, -1.000000000000000000 ) ) ;
#23615 = AXIS2_PLACEMENT_3D ( 'NONE', #16955, #2072, #5628 ) ;
#23616 = AXIS2_PLACEMENT_3D ( 'NONE', #62, #18138, #12850 ) ;
#23617 = ORIENTED_EDGE ( 'NONE', *, *, #17469, .T. ) ;
#23618 = VECTOR ( 'NONE', #22216, 1000.000000000000000 ) ;
#23619 = ORIENTED_EDGE ( 'NONE', *, *, #6826, .F. ) ;
#23620 = ORIENTED_EDGE ( 'NONE', *, *, #4260, .F. ) ;
#23621 = ORIENTED_EDGE ( 'NONE', *, *, #5462, .F. ) ;
#23622 = DIRECTION ( 'NONE',  ( 1.000000000000000000, 0.000000000000000000, 0.000000000000000000 ) ) ;
#23623 = DIRECTION ( 'NONE',  ( 1.000000000000000000, 2.600433232233976523E-16, -0.000000000000000000 ) ) ;
#23624 = CARTESIAN_POINT ( 'NONE',  ( 0.000000000000000000, 0.000000000000000000, 0.000000000000000000 ) ) ;
#23625 = EDGE_LOOP ( 'NONE', ( #10036, #1061, #6096, #4932 ) ) ;
#23626 = DIRECTION ( 'NONE',  ( 1.000000000000000000, 0.000000000000000000, 0.000000000000000000 ) ) ;
#23627 = VECTOR ( 'NONE', #1387, 1000.000000000000000 ) ;
#23628 = DIRECTION ( 'NONE',  ( -1.000000000000000000, -0.000000000000000000, -0.000000000000000000 ) ) ;
#23629 = ORIENTED_EDGE ( 'NONE', *, *, #19883, .T. ) ;
#23630 = CARTESIAN_POINT ( 'NONE',  ( 23.00000000000000000, -13.66196005206961850, -3.918670437617226110 ) ) ;
#23631 = CARTESIAN_POINT ( 'NONE',  ( 0.000000000000000000, 0.000000000000000000, 0.000000000000000000 ) ) ;
#23632 = EDGE_CURVE ( 'NONE', #4705, #19429, #9566, .T. ) ;
#23634 = CARTESIAN_POINT ( 'NONE',  ( 41.00000000000000000, -5.000000000000015099, 10.49999999999999822 ) ) ;
#23633 = AXIS2_PLACEMENT_3D ( 'NONE', #9125, #8636, #18294 ) ;
#23635 = DIRECTION ( 'NONE',  ( -0.000000000000000000, -0.000000000000000000, -1.000000000000000000 ) ) ;
#23636 = CARTESIAN_POINT ( 'NONE',  ( 2.935661446561383503, 9.035036904804158553, 4.459589141758144137 ) ) ;
#23637 = EDGE_CURVE ( 'NONE', #12337, #12612, #6280, .T. ) ;
#23638 = VECTOR ( 'NONE', #18339, 1000.000000000000114 ) ;
#23639 = CARTESIAN_POINT ( 'NONE',  ( 16.44572538483723179, -6.755397553796130161, -6.683320200552548052 ) ) ;
#23640 = LINE ( 'NONE', #19956, #5215 ) ;
#23641 = EDGE_CURVE ( 'NONE', #9464, #5416, #21174, .T. ) ;
#23642 = CARTESIAN_POINT ( 'NONE',  ( 43.50000000000000711, 25.22443390181681622, -1.500000000000000000 ) ) ;
#23643 = EDGE_CURVE ( 'NONE', #1246, #23953, #22075, .T. ) ;
#23644 = DIRECTION ( 'NONE',  ( -1.000000000000000000, -1.224606353822377258E-16, -0.000000000000000000 ) ) ;
#23645 = ORIENTED_EDGE ( 'NONE', *, *, #15502, .T. ) ;
#23646 = CARTESIAN_POINT ( 'NONE',  ( -5.365059087798939252, -7.384370330707086261, 3.933165578109188321 ) ) ;
#23647 = CIRCLE ( 'NONE', #8019, 1.000000000000000888 ) ;
#23648 = CARTESIAN_POINT ( 'NONE',  ( 2.454813078130514813E-15, 16.67999999999999972, 13.00000000000000178 ) ) ;
#23649 = AXIS2_PLACEMENT_3D ( 'NONE', #17793, #23030, #8379 ) ;
#23650 = ORIENTED_EDGE ( 'NONE', *, *, #17495, .F. ) ;
#23651 = CARTESIAN_POINT ( 'NONE',  ( 30.68762588338046982, -45.64284848299539732, -3.000000000000000000 ) ) ;
#23652 = CARTESIAN_POINT ( 'NONE',  ( 2.935661446562616295, -9.035036904803758873, -7.659589141758144315 ) ) ;
#23653 = AXIS2_PLACEMENT_3D ( 'NONE', #21267, #19434, #19685 ) ;
#23654 = DIRECTION ( 'NONE',  ( 0.000000000000000000, 0.000000000000000000, 1.000000000000000000 ) ) ;
#23655 = FACE_OUTER_BOUND ( 'NONE', #9210, .T. ) ;
#23656 = CARTESIAN_POINT ( 'NONE',  ( -6.153822176767817416E-13, 9.500000000000000000, 3.637828009640154736 ) ) ;
#23657 = CARTESIAN_POINT ( 'NONE',  ( 29.99999999999998934, -1.387778780781445676E-14, 10.49999999999999822 ) ) ;
#23658 = ORIENTED_EDGE ( 'NONE', *, *, #12914, .T. ) ;
#23659 = CARTESIAN_POINT ( 'NONE',  ( 1.224646799147352468E-16, -12.99147757894464306, 8.749999999999998224 ) ) ;
#23660 = EDGE_CURVE ( 'NONE', #11172, #5011, #11942, .T. ) ;
#23661 = ORIENTED_EDGE ( 'NONE', *, *, #12674, .T. ) ;
#23662 = CIRCLE ( 'NONE', #22488, 5.000000000000007994 ) ;
#23663 = CARTESIAN_POINT ( 'NONE',  ( 2.024999999999999911, -45.00000000000000000, 0.000000000000000000 ) ) ;
#23664 = CARTESIAN_POINT ( 'NONE',  ( 65.27272727272728048, -4.172000000000000597, 5.616230220889771312E-16 ) ) ;
#23665 = CARTESIAN_POINT ( 'NONE',  ( 0.000000000000000000, 0.000000000000000000, -2.500000000000000000 ) ) ;
#23666 = EDGE_CURVE ( 'NONE', #7845, #886, #13111, .T. ) ;
#23667 = DIRECTION ( 'NONE',  ( 0.5735764363510424957, 0.8191520442889943521, 0.000000000000000000 ) ) ;
#23668 = ADVANCED_FACE ( 'NONE', ( #9796 ), #16992, .T. ) ;
#23669 = ORIENTED_EDGE ( 'NONE', *, *, #13025, .T. ) ;
#23670 = DIRECTION ( 'NONE',  ( 0.000000000000000000, 1.000000000000000000, 0.000000000000000000 ) ) ;
#23671 = ADVANCED_FACE ( 'NONE', ( #6168 ), #12336, .T. ) ;
#23672 = EDGE_CURVE ( 'NONE', #13956, #9630, #20140, .T. ) ;
#23673 = DIRECTION ( 'NONE',  ( 0.000000000000000000, 0.000000000000000000, -1.000000000000000000 ) ) ;
#23674 = ORIENTED_EDGE ( 'NONE', *, *, #23958, .T. ) ;
#23675 = VERTEX_POINT ( 'NONE', #929 ) ;
#23676 = CARTESIAN_POINT ( 'NONE',  ( -9.499999999999790390, -3.086737114213257804, 12.30674201446023197 ) ) ;
#23677 = FACE_OUTER_BOUND ( 'NONE', #14066, .T. ) ;
#23678 = ORIENTED_EDGE ( 'NONE', *, *, #9628, .T. ) ;
#23679 = DIRECTION ( 'NONE',  ( -1.000000000000000000, 0.000000000000000000, -0.000000000000000000 ) ) ;
#23680 = CARTESIAN_POINT ( 'NONE',  ( 39.99999999999999289, 29.50000000000000000, 27.00000000000000000 ) ) ;
#23681 = DIRECTION ( 'NONE',  ( 1.000000000000000000, 0.000000000000000000, 0.000000000000000000 ) ) ;
#23682 = SURFACE_SIDE_STYLE ('',( #10481 ) ) ;
#23683 = DIRECTION ( 'NONE',  ( -0.000000000000000000, 1.000000000000000000, -0.000000000000000000 ) ) ;
#23684 = PRODUCT ( 'Oil seal', 'Oil seal', '', ( #19968 ) ) ;
#23685 = DIRECTION ( 'NONE',  ( 0.000000000000000000, 1.000000000000000000, 0.000000000000000000 ) ) ;
#23686 = EDGE_CURVE ( 'NONE', #13385, #2874, #563, .T. ) ;
#23687 = EDGE_LOOP ( 'NONE', ( #7346, #3594 ) ) ;
#23688 = DIRECTION ( 'NONE',  ( -0.000000000000000000, -0.000000000000000000, 1.000000000000000000 ) ) ;
#23689 = CARTESIAN_POINT ( 'NONE',  ( 76.90909090909090651, 7.491529369508391930E-15, 0.000000000000000000 ) ) ;
#23690 = CARTESIAN_POINT ( 'NONE',  ( -4.199395741333246335, 8.543843702856307232, -3.498976002706156496 ) ) ;
#23691 = DIRECTION ( 'NONE',  ( 0.000000000000000000, -1.000000000000000000, 0.000000000000000000 ) ) ;
#23692 = EDGE_CURVE ( 'NONE', #11303, #1974, #17407, .T. ) ;
#23693 = DIRECTION ( 'NONE',  ( 0.000000000000000000, -0.000000000000000000, -1.000000000000000000 ) ) ;
#23694 = ORIENTED_EDGE ( 'NONE', *, *, #3936, .F. ) ;
#23695 = CARTESIAN_POINT ( 'NONE',  ( 8.680847955711007202, 5.912916378492122225E-13, -10.63316557810918894 ) ) ;
#23696 = EDGE_CURVE ( 'NONE', #16661, #14137, #13305, .T. ) ;
#23697 = DIRECTION ( 'NONE',  ( -0.000000000000000000, -0.000000000000000000, -1.000000000000000000 ) ) ;
#23698 = ORIENTED_EDGE ( 'NONE', *, *, #7913, .T. ) ;
#23699 = DIRECTION ( 'NONE',  ( 0.000000000000000000, 0.000000000000000000, 1.000000000000000000 ) ) ;
#23700 = VERTEX_POINT ( 'NONE', #13444 ) ;
#23701 = DIRECTION ( 'NONE',  ( -0.000000000000000000, -0.000000000000000000, -1.000000000000000000 ) ) ;
#23702 = ORIENTED_EDGE ( 'NONE', *, *, #9942, .T. ) ;
#23703 = CARTESIAN_POINT ( 'NONE',  ( 20.85000000000000497, 16.67999999999999972, 14.50000000000000000 ) ) ;
#23704 = DIRECTION ( 'NONE',  ( 0.000000000000000000, -0.5406408174555871193, -0.8412535328311879779 ) ) ;
#23705 = CARTESIAN_POINT ( 'NONE',  ( 73.12522638709218370, 7.562528597612068045E-15, 0.000000000000000000 ) ) ;
#23706 = VERTEX_POINT ( 'NONE', #7570 ) ;
#23707 = DIRECTION ( 'NONE',  ( 1.000000000000000000, 0.000000000000000000, 0.000000000000000000 ) ) ;
#23708 = CARTESIAN_POINT ( 'NONE',  ( 1.999999999999996669, -45.00000000000000000, -8.673617379884035472E-16 ) ) ;
#23709 = CARTESIAN_POINT ( 'NONE',  ( 9.499999999999790390, 3.086737114213260025, -5.306742014460231971 ) ) ;
#23710 = VERTEX_POINT ( 'NONE', #15017 ) ;
#23711 = ORIENTED_EDGE ( 'NONE', *, *, #16794, .F. ) ;
#23712 = FACE_OUTER_BOUND ( 'NONE', #4557, .T. ) ;
#23713 = DIRECTION ( 'NONE',  ( 0.000000000000000000, 0.000000000000000000, 1.000000000000000000 ) ) ;
#23714 = ADVANCED_FACE ( 'NONE', ( #20646 ), #9982, .T. ) ;
#23715 = PLANE ( 'NONE',  #3821 ) ;
#23716 = ORIENTED_EDGE ( 'NONE', *, *, #12876, .T. ) ;
#23717 = EDGE_CURVE ( 'NONE', #21492, #18499, #14287, .T. ) ;
#23718 = CARTESIAN_POINT ( 'NONE',  ( -1.749335460928132413, -9.337549220493531976, -3.500000000000076383 ) ) ;
#23719 = CYLINDRICAL_SURFACE ( 'NONE', #9084, 40.00000000000000000 ) ;
#23720 = ORIENTED_EDGE ( 'NONE', *, *, #7354, .T. ) ;
#23721 = DIRECTION ( 'NONE',  ( -1.000000000000000000, -1.224606353822377258E-16, -0.000000000000000000 ) ) ;
#23722 = DIRECTION ( 'NONE',  ( -1.000000000000000000, 2.600433232233976523E-16, 0.000000000000000000 ) ) ;
#23723 = CARTESIAN_POINT ( 'NONE',  ( 1.999999999999994449, -45.00000000000000000, -26.97499999999999432 ) ) ;
#23724 = CARTESIAN_POINT ( 'NONE',  ( 9.500000000000209610, -3.086737114211962396, 3.959589141758145026 ) ) ;
#23725 = AXIS2_PLACEMENT_3D ( 'NONE', #502, #9997, #21000 ) ;
#23726 = ORIENTED_EDGE ( 'NONE', *, *, #21007, .T. ) ;
#23727 = ORIENTED_EDGE ( 'NONE', *, *, #15188, .T. ) ;
#23728 = B_SPLINE_CURVE_WITH_KNOTS ( 'NONE', 3,
 ( #5726, #828, #13756, #594, #7761, #21205, #6082, #9710, #2541, #15195, #17290, #11658, #19129, #11551 ),
 .UNSPECIFIED., .F., .F.,
 ( 4, 2, 2, 2, 2, 2, 4 ),
 ( 4.128177188600459851E-16, 0.001553140985941505034, 0.002329711478912049709, 0.003106281971882594601, 0.004659422957823682217, 0.005435993450794225808, 0.006212563943764767664 ),
 .UNSPECIFIED. ) ;
#23729 = EDGE_LOOP ( 'NONE', ( #13470, #10580 ) ) ;
#23730 = CARTESIAN_POINT ( 'NONE',  ( -28.00000000000000355, -51.00000000000000711, 0.5000000000000000000 ) ) ;
#23731 = AXIS2_PLACEMENT_3D ( 'NONE', #19168, #11587, #22706 ) ;
#23732 = EDGE_CURVE ( 'NONE', #21692, #23700, #10754, .T. ) ;
#23733 = CARTESIAN_POINT ( 'NONE',  ( 0.000000000000000000, -1.934484387511856252, -14.08058594723508072 ) ) ;
#23734 = DIRECTION ( 'NONE',  ( -1.000000000000000000, -0.000000000000000000, 0.000000000000000000 ) ) ;
#23735 = ORIENTED_EDGE ( 'NONE', *, *, #3892, .T. ) ;
#23736 = EDGE_CURVE ( 'NONE', #11854, #13833, #7634, .T. ) ;
#23737 = CARTESIAN_POINT ( 'NONE',  ( 86.21613547800127719, -5.000000000000000000, 6.123233995736775157E-16 ) ) ;
#23738 = ORIENTED_EDGE ( 'NONE', *, *, #8520, .T. ) ;
#23739 = CARTESIAN_POINT ( 'NONE',  ( 0.000000000000000000, 0.000000000000000000, 0.000000000000000000 ) ) ;
#23740 = VECTOR ( 'NONE', #10243, 1000.000000000000000 ) ;
#23741 = SHAPE_REPRESENTATION ( 'Part11^Assembly Idle gear', ( #8005 ), #2575 ) ;
#23742 = CARTESIAN_POINT ( 'NONE',  ( 20.99999999999999645, 29.50000000000000355, 12.00000000000000000 ) ) ;
#23743 = EDGE_CURVE ( 'NONE', #11720, #13291, #18696, .T. ) ;
#23744 = CARTESIAN_POINT ( 'NONE',  ( -1.504652183083727168, 9.499999999999904077, 3.757996296007079184 ) ) ;
#23745 = DIRECTION ( 'NONE',  ( 1.000000000000000000, 0.000000000000000000, 0.000000000000000000 ) ) ;
#23746 = DIRECTION ( 'NONE',  ( -0.000000000000000000, -0.000000000000000000, -1.000000000000000000 ) ) ;
#23747 = CARTESIAN_POINT ( 'NONE',  ( 81.85249911436491743, 5.000000000000015099, 0.000000000000000000 ) ) ;
#23748 = FACE_OUTER_BOUND ( 'NONE', #9391, .T. ) ;
#23749 = CARTESIAN_POINT ( 'NONE',  ( 0.000000000000000000, -14.99147757894464306, 6.724999999999999645 ) ) ;
#23750 = CARTESIAN_POINT ( 'NONE',  ( -0.9830802669677229932, 45.00000000000000000, 3.000000000000002665 ) ) ;
#23751 = CARTESIAN_POINT ( 'NONE',  ( 10.00000000000000000, 0.000000000000000000, -5.400000000000001243 ) ) ;
#23752 = CARTESIAN_POINT ( 'NONE',  ( 2.682529543900284974, -8.255977015246234174, 10.23316557810918859 ) ) ;
#23753 = VERTEX_POINT ( 'NONE', #16732 ) ;
#23754 = PRODUCT_CONTEXT ( 'NONE', #3548, 'mechanical' ) ;
#23755 = DIRECTION ( 'NONE',  ( 1.000000000000000000, 0.000000000000000000, -0.000000000000000000 ) ) ;
#23756 = VERTEX_POINT ( 'NONE', #11332 ) ;
#23757 = CARTESIAN_POINT ( 'NONE',  ( -9.209619485559194629, 2.039334951465706869, -12.08108701042788979 ) ) ;
#23758 = CARTESIAN_POINT ( 'NONE',  ( -7.685661446561619314, -5.583959896779019161, -9.259589141758143072 ) ) ;
#23759 = DIRECTION ( 'NONE',  ( -1.000000000000000000, -0.000000000000000000, -0.000000000000000000 ) ) ;
#23760 = DIRECTION ( 'NONE',  ( 0.000000000000000000, 0.000000000000000000, 1.000000000000000000 ) ) ;
#23761 = DIRECTION ( 'NONE',  ( -1.000000000000000000, 0.000000000000000000, 0.000000000000000000 ) ) ;
#23762 = EDGE_CURVE ( 'NONE', #18287, #23864, #22856, .T. ) ;
#23763 = ADVANCED_FACE ( 'NONE', ( #22601 ), #18593, .T. ) ;
#23764 = CARTESIAN_POINT ( 'NONE',  ( -41.73082370883260239, 27.62204025492845361, -1.500000000000000000 ) ) ;
#23765 = ORIENTED_EDGE ( 'NONE', *, *, #17328, .T. ) ;
#23766 = FACE_OUTER_BOUND ( 'NONE', #23001, .T. ) ;
#23767 = VECTOR ( 'NONE', #12847, 1000.000000000000227 ) ;
#23768 = DIRECTION ( 'NONE',  ( -1.000000000000000000, 0.000000000000000000, 0.000000000000000000 ) ) ;
#23769 = PLANE ( 'NONE',  #22690 ) ;
#23770 = LINE ( 'NONE', #5221, #15702 ) ;
#23771 = CARTESIAN_POINT ( 'NONE',  ( 0.000000000000000000, -15.03999999999999915, 25.00000000000000000 ) ) ;
#23772 = VERTEX_POINT ( 'NONE', #6006 ) ;
#23773 = PLANE ( 'NONE',  #9428 ) ;
#23774 = ORIENTED_EDGE ( 'NONE', *, *, #5470, .T. ) ;
#23775 = VERTEX_POINT ( 'NONE', #13571 ) ;
#23776 = CARTESIAN_POINT ( 'NONE',  ( -5.871322893124554021, 8.081182679343978492, 9.906742014460235168 ) ) ;
#23777 = CARTESIAN_POINT ( 'NONE',  ( -9.500000000000211386, 3.086737114211961064, 6.106742014460234458 ) ) ;
#23778 = VERTEX_POINT ( 'NONE', #19066 ) ;
#23779 = ORIENTED_EDGE ( 'NONE', *, *, #7444, .T. ) ;
#23780 = EDGE_CURVE ( 'NONE', #12468, #8700, #1829, .T. ) ;
#23781 = CARTESIAN_POINT ( 'NONE',  ( -37.00000000000000711, 29.49999999999999645, 11.50000000000000000 ) ) ;
#23782 = DIRECTION ( 'NONE',  ( 0.000000000000000000, 0.000000000000000000, 1.000000000000000000 ) ) ;
#23783 = CARTESIAN_POINT ( 'NONE',  ( -36.00000000000001421, 50.99999999999999289, 12.50000000000000000 ) ) ;
#23784 = CARTESIAN_POINT ( 'NONE',  ( 2.935661446562616295, -9.035036904803758873, -4.806742014460232859 ) ) ;
#23785 = FACE_OUTER_BOUND ( 'NONE', #13775, .T. ) ;
#23786 = LINE ( 'NONE', #10719, #10975 ) ;
#23787 = ADVANCED_FACE ( 'NONE', ( #5877 ), #16242, .T. ) ;
#23788 = EDGE_CURVE ( 'NONE', #978, #6856, #15844, .T. ) ;
#23789 = DIRECTION ( 'NONE',  ( -0.000000000000000000, -0.000000000000000000, -1.000000000000000000 ) ) ;
#23790 = EDGE_LOOP ( 'NONE', ( #4153, #1108, #14384, #11246 ) ) ;
#23791 = CARTESIAN_POINT ( 'NONE',  ( -40.66734255040736201, -26.56420859267092283, -3.000000000000000000 ) ) ;
#23792 = ORIENTED_EDGE ( 'NONE', *, *, #18278, .T. ) ;
#23793 = CARTESIAN_POINT ( 'NONE',  ( -12.50000000000000178, 1.672973214995343413E-15, 2.500000000000000000 ) ) ;
#23794 = CARTESIAN_POINT ( 'NONE',  ( -41.00000000000000000, -4.000000000000000888, 10.49999999999999822 ) ) ;
#23795 = CARTESIAN_POINT ( 'NONE',  ( -6.153822176767817416E-13, 9.500000000000000000, -3.500000000000014211 ) ) ;
#23796 = CARTESIAN_POINT ( 'NONE',  ( 79.23840997654417606, 6.123233995736675563E-16, -5.000000000000007994 ) ) ;
#23797 = AXIS2_PLACEMENT_3D ( 'NONE', #22192, #7171, #1569 ) ;
#23798 = DIRECTION ( 'NONE',  ( 0.5735764363510427177, -0.8191520442889941300, 1.003171929053527705E-16 ) ) ;
#23799 = CARTESIAN_POINT ( 'NONE',  ( 7.022953521755574080, -5.102474405759714671, -8.433165578109187877 ) ) ;
#23800 = CARTESIAN_POINT ( 'NONE',  ( -14.91530227160598265, 1.623290104782663335, 9.365835742197235803 ) ) ;
#23801 = ORIENTED_EDGE ( 'NONE', *, *, #21102, .T. ) ;
#23802 = DIRECTION ( 'NONE',  ( -0.000000000000000000, -0.000000000000000000, -1.000000000000000000 ) ) ;
#23803 = VERTEX_POINT ( 'NONE', #17093 ) ;
#23804 = CARTESIAN_POINT ( 'NONE',  ( -41.49999999999999289, -27.79189783386527779, 27.00000000000000000 ) ) ;
#23805 = DIRECTION ( 'NONE',  ( 0.000000000000000000, -1.000000000000000000, 0.000000000000000000 ) ) ;
#23806 = ORIENTED_EDGE ( 'NONE', *, *, #166, .T. ) ;
#23807 = CARTESIAN_POINT ( 'NONE',  ( -34.00000000000000000, -3.851859888774471706E-31, 10.49999999999999822 ) ) ;
#23808 = ADVANCED_FACE ( 'NONE', ( #396 ), #18962, .T. ) ;
#23809 = CARTESIAN_POINT ( 'NONE',  ( -7.685661446562381371, 5.583959896777970222, -2.859589141758144493 ) ) ;
#23810 = CARTESIAN_POINT ( 'NONE',  ( 81.85249911436491743, 5.000000000000015987, 0.000000000000000000 ) ) ;
#23811 = DIRECTION ( 'NONE',  ( -0.000000000000000000, -0.000000000000000000, -1.000000000000000000 ) ) ;
#23812 = ADVANCED_FACE ( 'NONE', ( #7934 ), #9287, .F. ) ;
#23813 = CARTESIAN_POINT ( 'NONE',  ( -34.00000000000000000, -3.851859888774471706E-31, 10.49999999999999822 ) ) ;
#23814 = ADVANCED_FACE ( 'NONE', ( #13075 ), #20542, .T. ) ;
#23815 = CARTESIAN_POINT ( 'NONE',  ( -2.935661446562617183, 9.035036904803758873, -5.806742014460233747 ) ) ;
#23816 = EDGE_LOOP ( 'NONE', ( #126, #12597, #1441 ) ) ;
#23817 = ORIENTED_EDGE ( 'NONE', *, *, #15769, .F. ) ;
#23818 = DIRECTION ( 'NONE',  ( -1.000000000000000000, 0.000000000000000000, 0.000000000000000000 ) ) ;
#23819 = DIRECTION ( 'NONE',  ( -0.000000000000000000, -0.000000000000000000, -1.000000000000000000 ) ) ;
#23820 = ORIENTED_EDGE ( 'NONE', *, *, #2232, .T. ) ;
#23821 = DIRECTION ( 'NONE',  ( -0.000000000000000000, -0.000000000000000000, 1.000000000000000000 ) ) ;
#23822 = DIRECTION ( 'NONE',  ( 0.000000000000000000, 0.000000000000000000, -1.000000000000000000 ) ) ;
#23823 = AXIS2_PLACEMENT_3D ( 'NONE', #5295, #5167, #1627 ) ;
#23824 = VERTEX_POINT ( 'NONE', #21382 ) ;
#23825 =( REPRESENTATION_RELATIONSHIP ('NONE','NONE', #12815, #358 ) REPRESENTATION_RELATIONSHIP_WITH_TRANSFORMATION ( #13577 )SHAPE_REPRESENTATION_RELATIONSHIP( ) );
#23826 = FACE_OUTER_BOUND ( 'NONE', #23573, .T. ) ;
#23827 = LINE ( 'NONE', #14418, #11773 ) ;
#23828 = CARTESIAN_POINT ( 'NONE',  ( 23.85000000000000142, 15.03999999999999737, 2.200000000000000178 ) ) ;
#23829 = CONICAL_SURFACE ( 'NONE', #13272, 1.999999999999994449, 1.029744258676653201 ) ;
#23830 = CARTESIAN_POINT ( 'NONE',  ( 14.51962751333974389, 3.765689428759029234, 27.00000000000000000 ) ) ;
#23831 = ORIENTED_EDGE ( 'NONE', *, *, #1808, .T. ) ;
#23832 = ORIENTED_EDGE ( 'NONE', *, *, #6348, .F. ) ;
#23833 = ORIENTED_EDGE ( 'NONE', *, *, #4574, .T. ) ;
#23834 = LINE ( 'NONE', #4958, #18572 ) ;
#23835 = ADVANCED_FACE ( 'NONE', ( #21497 ), #2466, .F. ) ;
#23836 = LINE ( 'NONE', #1419, #22342 ) ;
#23837 = ORIENTED_EDGE ( 'NONE', *, *, #9142, .T. ) ;
#23838 = CONICAL_SURFACE ( 'NONE', #14469, 1.999999999999994449, 1.029744258676653201 ) ;
#23839 = DIRECTION ( 'NONE',  ( 0.000000000000000000, -0.9898214418809341275, 0.1423148382732755679 ) ) ;
#23840 = DIRECTION ( 'NONE',  ( -0.000000000000000000, -0.000000000000000000, -1.000000000000000000 ) ) ;
#23841 = AXIS2_PLACEMENT_3D ( 'NONE', #3832, #16523, #16648 ) ;
#23842 = ORIENTED_EDGE ( 'NONE', *, *, #19958, .F. ) ;
#23843 = LINE ( 'NONE', #14433, #11116 ) ;
#23844 = DIRECTION ( 'NONE',  ( 1.000000000000000000, 0.000000000000000000, 0.000000000000000000 ) ) ;
#23845 = CARTESIAN_POINT ( 'NONE',  ( 89.12522638709219791, -5.000000000000000000, 6.123233995736775157E-16 ) ) ;
#23846 = CARTESIAN_POINT ( 'NONE',  ( -42.00000000000000000, -26.82133436441678853, 0.000000000000000000 ) ) ;
#23847 = CARTESIAN_POINT ( 'NONE',  ( 6.809999908187194197E-13, -9.988891130263535700, 10.70674201446023410 ) ) ;
#23848 = DIRECTION ( 'NONE',  ( -0.000000000000000000, -0.000000000000000000, -1.000000000000000000 ) ) ;
#23849 = CYLINDRICAL_SURFACE ( 'NONE', #20381, 8.000000000000000000 ) ;
#23850 = EDGE_CURVE ( 'NONE', #1523, #1617, #10007, .T. ) ;
#23851 = CARTESIAN_POINT ( 'NONE',  ( -14.79227890392045275, 2.568991289487078333, -9.169086800441911933 ) ) ;
#23852 = CARTESIAN_POINT ( 'NONE',  ( -7.022953521754877748, -5.102474405760673015, 9.833165578109188232 ) ) ;
#23853 = ORIENTED_EDGE ( 'NONE', *, *, #10545, .F. ) ;
#23854 = VECTOR ( 'NONE', #5217, 999.9999999999998863 ) ;
#23855 = CIRCLE ( 'NONE', #13319, 8.000000000000000000 ) ;
#23856 = EDGE_CURVE ( 'NONE', #12216, #8851, #22097, .T. ) ;
#23857 = CIRCLE ( 'NONE', #488, 11.00000000000000711 ) ;
#23858 = AXIS2_PLACEMENT_3D ( 'NONE', #13902, #5966, #9610 ) ;
#23859 = VECTOR ( 'NONE', #19527, 1000.000000000000000 ) ;
#23860 = CARTESIAN_POINT ( 'NONE',  ( 649.2818939062883601, 888.4837211537977737, 1320.481724745927750 ) ) ;
#23861 = VECTOR ( 'NONE', #20792, 1000.000000000000000 ) ;
#23862 = EDGE_CURVE ( 'NONE', #20276, #18514, #11539, .T. ) ;
#23863 = VECTOR ( 'NONE', #20645, 1000.000000000000000 ) ;
#23864 = VERTEX_POINT ( 'NONE', #15886 ) ;
#23865 = ORIENTED_EDGE ( 'NONE', *, *, #22445, .F. ) ;
#23866 = EDGE_CURVE ( 'NONE', #23824, #10172, #2999, .T. ) ;
#23867 = CARTESIAN_POINT ( 'NONE',  ( -9.355838966532735057, 1.029750461815885476, -12.10148668281140871 ) ) ;
#23868 = CARTESIAN_POINT ( 'NONE',  ( -2.935661446562617183, 9.035036904803758873, -6.659589141758144315 ) ) ;
#23869 =( BOUNDED_CURVE ( )  B_SPLINE_CURVE ( 2, ( #3997, #7873, #6197, #11418, #22800, #19385, #17531, #19259, #20713, #6306, #15697 ),
 .UNSPECIFIED., .F., .T. ) 
 B_SPLINE_CURVE_WITH_KNOTS ( ( 3, 2, 2, 2, 2, 3 ),
 ( 0.2000000000000000111, 0.2200000000000000289, 0.2400000000000000466, 0.2600000000000000644, 0.2800000000000001377, 0.3000000000000000999 ),
 .UNSPECIFIED. ) 
 CURVE ( )  GEOMETRIC_REPRESENTATION_ITEM ( )  RATIONAL_B_SPLINE_CURVE ( ( 1.000000000000000000, 0.9510565162951535312, 1.000000000000000000, 0.9510565162951535312, 1.000000000000000000, 0.9510565162951535312, 1.000000000000000000, 0.9510565162951535312, 1.000000000000000000, 0.9510565162951533091, 1.000000000000000222 ) ) 
 REPRESENTATION_ITEM ( '' )  );
#23870 = CARTESIAN_POINT ( 'NONE',  ( 23.00000000000000000, 0.000000000000000000, 0.000000000000000000 ) ) ;
#23871 = DIRECTION ( 'NONE',  ( 0.000000000000000000, 0.000000000000000000, 1.000000000000000000 ) ) ;
#23872 = CARTESIAN_POINT ( 'NONE',  ( -8.000000000000000000, 9.797174393178825657E-16, 12.50000000000000000 ) ) ;
#23873 = FACE_OUTER_BOUND ( 'NONE', #4140, .T. ) ;
#23874 = ORIENTED_EDGE ( 'NONE', *, *, #24078, .T. ) ;
#23875 = CARTESIAN_POINT ( 'NONE',  ( 9.500000000000200728, -3.086737114211976607, -7.106742014460232681 ) ) ;
#23876 = VECTOR ( 'NONE', #17800, 1000.000000000000000 ) ;
#23877 = VECTOR ( 'NONE', #6335, 1000.000000000000000 ) ;
#23878 = CARTESIAN_POINT ( 'NONE',  ( 67.30704456891035647, -1.078520768856852078E-29, 5.000000000000007994 ) ) ;
#23879 = CARTESIAN_POINT ( 'NONE',  ( 57.42022815836235594, 7.420530141404717394E-15, 0.000000000000000000 ) ) ;
#23880 = AXIS2_PLACEMENT_3D ( 'NONE', #22899, #17262, #6169 ) ;
#23881 = VECTOR ( 'NONE', #10301, 1000.000000000000000 ) ;
#23882 = FACE_OUTER_BOUND ( 'NONE', #15880, .T. ) ;
#23883 = FILL_AREA_STYLE ('',( #9231 ) ) ;
#23884 = CIRCLE ( 'NONE', #7480, 11.23082370883260417 ) ;
#23885 = CIRCLE ( 'NONE', #5579, 11.24716442891539714 ) ;
#23886 = DIRECTION ( 'NONE',  ( -0.000000000000000000, -0.000000000000000000, -1.000000000000000000 ) ) ;
#23887 = EDGE_LOOP ( 'NONE', ( #23738, #17673, #3930, #22521 ) ) ;
#23888 = DIRECTION ( 'NONE',  ( 0.000000000000000000, 1.224646799147353207E-16, 1.000000000000000000 ) ) ;
#23890 = EDGE_CURVE ( 'NONE', #5210, #3315, #7267, .T. ) ;
#23889 = CARTESIAN_POINT ( 'NONE',  ( -2.935661446561384391, -9.035036904804158553, -10.60674201446023446 ) ) ;
#23891 = AXIS2_PLACEMENT_3D ( 'NONE', #16890, #7842, #11257 ) ;
#23892 = DIRECTION ( 'NONE',  ( -1.000000000000000000, 0.000000000000000000, 0.000000000000000000 ) ) ;
#23893 = ORIENTED_EDGE ( 'NONE', *, *, #1162, .F. ) ;
#23894 = ORIENTED_EDGE ( 'NONE', *, *, #13182, .F. ) ;
#23895 = CARTESIAN_POINT ( 'NONE',  ( -2.935661446562617183, 9.035036904803758873, 11.80674201446023375 ) ) ;
#23896 = EDGE_CURVE ( 'NONE', #18951, #3309, #20913, .T. ) ;
#23897 = CARTESIAN_POINT ( 'NONE',  ( -7.685661446561619314, -5.583959896779019161, 6.406742014460233392 ) ) ;
#23898 = CARTESIAN_POINT ( 'NONE',  ( 0.000000000000000000, -14.99147757894464306, 7.750000000000000000 ) ) ;
#23899 = ORIENTED_EDGE ( 'NONE', *, *, #9092, .F. ) ;
#23900 = EDGE_CURVE ( 'NONE', #12989, #5706, #10386, .T. ) ;
#23901 = ORIENTED_EDGE ( 'NONE', *, *, #16791, .F. ) ;
#23902 = DIRECTION ( 'NONE',  ( 5.886191147978116460E-17, 1.967575324405878944E-17, -0.9999999999999997780 ) ) ;
#23903 = CARTESIAN_POINT ( 'NONE',  ( -19.84999999999999787, -16.67999999999984695, 14.50000000000000000 ) ) ;
#23904 = VECTOR ( 'NONE', #19478, 1000.000000000000000 ) ;
#23905 = AXIS2_PLACEMENT_3D ( 'NONE', #19767, #14246, #21591 ) ;
#23906 = DIRECTION ( 'NONE',  ( -0.000000000000000000, -0.000000000000000000, -1.000000000000000000 ) ) ;
#23907 = AXIS2_PLACEMENT_3D ( 'NONE', #5420, #7594, #416 ) ;
#23908 = VECTOR ( 'NONE', #21555, 1000.000000000000000 ) ;
#23909 = CIRCLE ( 'NONE', #18081, 9.999999999999998224 ) ;
#23910 = CARTESIAN_POINT ( 'NONE',  ( 84.76159002345582394, 7.562528597612068045E-15, 0.000000000000000000 ) ) ;
#23911 = CARTESIAN_POINT ( 'NONE',  ( 40.49999999999998579, -51.00000000000000711, 12.50000000000000000 ) ) ;
#23912 = DIRECTION ( 'NONE',  ( 0.000000000000000000, -1.000000000000000000, 0.000000000000000000 ) ) ;
#23913 = AXIS2_PLACEMENT_3D ( 'NONE', #16928, #3413, #1704 ) ;
#23914 = DIRECTION ( 'NONE',  ( 1.000000000000000000, 0.000000000000000000, 0.000000000000000000 ) ) ;
#23915 = DIRECTION ( 'NONE',  ( 0.000000000000000000, -1.000000000000000000, 0.000000000000000000 ) ) ;
#23916 = DIRECTION ( 'NONE',  ( -0.000000000000000000, -0.000000000000000000, -1.000000000000000000 ) ) ;
#23917 = DIRECTION ( 'NONE',  ( -0.000000000000000000, 1.000000000000000000, 0.000000000000000000 ) ) ;
#23918 = CIRCLE ( 'NONE', #16873, 5.000000000000007994 ) ;
#23919 = DIRECTION ( 'NONE',  ( -1.000000000000000000, -0.000000000000000000, -0.000000000000000000 ) ) ;
#23920 = VECTOR ( 'NONE', #5675, 1000.000000000000000 ) ;
#23921 = DIRECTION ( 'NONE',  ( 0.000000000000000000, 0.000000000000000000, 1.000000000000000000 ) ) ;
#23922 = VECTOR ( 'NONE', #22516, 1000.000000000000000 ) ;
#23923 = ADVANCED_FACE ( 'NONE', ( #764, #12075 ), #883, .T. ) ;
#23924 = ORIENTED_EDGE ( 'NONE', *, *, #5570, .F. ) ;
#23925 = DIRECTION ( 'NONE',  ( 1.000000000000000000, 0.000000000000000000, 0.000000000000000000 ) ) ;
#23926 = AXIS2_PLACEMENT_3D ( 'NONE', #14199, #7550, #10530 ) ;
#23927 = VERTEX_POINT ( 'NONE', #2958 ) ;
#23928 = CARTESIAN_POINT ( 'NONE',  ( 9.500000000000209610, -3.086737114211962396, -9.959589141758144137 ) ) ;
#23929 = EDGE_CURVE ( 'NONE', #10133, #2171, #6371, .T. ) ;
#23930 = AXIS2_PLACEMENT_3D ( 'NONE', #19242, #700, #15554 ) ;
#23931 = ADVANCED_FACE ( 'NONE', ( #15505 ), #8832, .F. ) ;
#23932 = VECTOR ( 'NONE', #11521, 1000.000000000000114 ) ;
#23933 = ORIENTED_EDGE ( 'NONE', *, *, #13931, .F. ) ;
#23934 = LINE ( 'NONE', #18568, #16818 ) ;
#23935 = AXIS2_PLACEMENT_3D ( 'NONE', #2186, #5737, #5969 ) ;
#23936 = CARTESIAN_POINT ( 'NONE',  ( 23.00000000000000000, -13.61176534793443338, -4.089617900950226925 ) ) ;
#23937 = VERTEX_POINT ( 'NONE', #8307 ) ;
#23938 = CARTESIAN_POINT ( 'NONE',  ( 31.49999999999999289, 50.99999999999999289, 0.5000000000000004441 ) ) ;
#23939 = DIRECTION ( 'NONE',  ( 0.000000000000000000, -1.000000000000000000, 0.000000000000000000 ) ) ;
#23940 = AXIS2_PLACEMENT_3D ( 'NONE', #1806, #18037, #7393 ) ;
#23941 = CARTESIAN_POINT ( 'NONE',  ( 9.499999999999790390, 3.086737114213260025, -10.15958914175814520 ) ) ;
#23942 = AXIS2_PLACEMENT_3D ( 'NONE', #7904, #17184, #4276 ) ;
#23943 = ORIENTED_EDGE ( 'NONE', *, *, #1498, .F. ) ;
#23944 = CYLINDRICAL_SURFACE ( 'NONE', #18489, 4.999999999999997335 ) ;
#23945 = FACE_OUTER_BOUND ( 'NONE', #21401, .T. ) ;
#23946 = AXIS2_PLACEMENT_3D ( 'NONE', #21759, #8918, #14772 ) ;
#23947 = CYLINDRICAL_SURFACE ( 'NONE', #12403, 5.000000000000000888 ) ;
#23948 = EDGE_CURVE ( 'NONE', #7640, #1246, #6897, .T. ) ;
#23949 = AXIS2_PLACEMENT_3D ( 'NONE', #8513, #12155, #10083 ) ;
#23950 = ORIENTED_EDGE ( 'NONE', *, *, #3888, .T. ) ;
#23951 = DIRECTION ( 'NONE',  ( -0.000000000000000000, 1.000000000000000000, -0.000000000000000000 ) ) ;
#23952 = DIRECTION ( 'NONE',  ( -0.000000000000000000, -0.000000000000000000, -1.000000000000000000 ) ) ;
#23953 = VERTEX_POINT ( 'NONE', #13682 ) ;
#23954 = CARTESIAN_POINT ( 'NONE',  ( -6.153822176767817416E-13, 9.500000000000000000, -2.873059427838766222 ) ) ;
#23955 = DIRECTION ( 'NONE',  ( 1.000000000000000000, 0.000000000000000000, 0.000000000000000000 ) ) ;
#23956 = EDGE_CURVE ( 'NONE', #1974, #19249, #23662, .T. ) ;
#23957 = FACE_OUTER_BOUND ( 'NONE', #1841, .T. ) ;
#23958 = EDGE_CURVE ( 'NONE', #12988, #15606, #23284, .T. ) ;
#23959 = CYLINDRICAL_SURFACE ( 'NONE', #5512, 50.00000000000000000 ) ;
#23960 = AXIS2_PLACEMENT_3D ( 'NONE', #222, #7501, #7631 ) ;
#23961 = CIRCLE ( 'NONE', #9912, 5.000000000000007994 ) ;
#23962 = ORIENTED_EDGE ( 'NONE', *, *, #15659, .T. ) ;
#23963 = CONICAL_SURFACE ( 'NONE', #5641, 1.999999999999994449, 1.029744258676653201 ) ;
#23964 = EDGE_LOOP ( 'NONE', ( #8317, #21926, #16862, #3683 ) ) ;
#23965 = AXIS2_PLACEMENT_3D ( 'NONE', #4714, #4478, #17139 ) ;
#23966 = ORIENTED_EDGE ( 'NONE', *, *, #21860, .T. ) ;
#23967 = DIRECTION ( 'NONE',  ( 0.000000000000000000, 0.000000000000000000, -1.000000000000000000 ) ) ;
#23968 = CIRCLE ( 'NONE', #14224, 5.000000000000000888 ) ;
#23969 = DIRECTION ( 'NONE',  ( -0.000000000000000000, -0.000000000000000000, 1.000000000000000000 ) ) ;
#23970 = DIRECTION ( 'NONE',  ( -1.000000000000000000, -0.000000000000000000, -0.000000000000000000 ) ) ;
#23971 = VERTEX_POINT ( 'NONE', #4430 ) ;
#23972 = ADVANCED_FACE ( 'NONE', ( #6617 ), #10260, .T. ) ;
#23973 = CARTESIAN_POINT ( 'NONE',  ( -7.866007474251193621, 5.334205555521198683, 12.00988687156538148 ) ) ;
#23974 = APPLICATION_CONTEXT ( 'automotive_design' ) ;
#23975 = DIRECTION ( 'NONE',  ( 0.000000000000000000, -1.000000000000000000, 0.000000000000000000 ) ) ;
#23976 = CARTESIAN_POINT ( 'NONE',  ( 23.85000000000000142, 15.03999999999999737, 2.200000000000000178 ) ) ;
#23977 = CARTESIAN_POINT ( 'NONE',  ( -31.10231664966676846, -45.36128193761570770, 12.00000000000000000 ) ) ;
#23978 = CIRCLE ( 'NONE', #7212, 3.000000000000002665 ) ;
#23979 = CIRCLE ( 'NONE', #1773, 2.024999999999999911 ) ;
#23980 = DIRECTION ( 'NONE',  ( 0.000000000000000000, -1.000000000000000000, 0.000000000000000000 ) ) ;
#23981 = DIRECTION ( 'NONE',  ( 1.000000000000000000, 0.000000000000000000, 0.000000000000000000 ) ) ;
#23982 = EDGE_LOOP ( 'NONE', ( #17220, #3336, #1022, #17402 ) ) ;
#23984 = ADVANCED_FACE ( 'NONE', ( #10124 ), #17576, .F. ) ;
#23983 = AXIS2_PLACEMENT_3D ( 'NONE', #20989, #11574, #13416 ) ;
#23985 = CARTESIAN_POINT ( 'NONE',  ( -5.365059087798939252, -7.384370330707086261, 11.93316557810918965 ) ) ;
#23986 = ORIENTED_EDGE ( 'NONE', *, *, #14745, .T. ) ;
#23987 = APPLICATION_PROTOCOL_DEFINITION ( 'draft international standard', 'automotive_design', 1998, #18992 ) ;
#23988 = DIRECTION ( 'NONE',  ( 0.8757121056631642642, -0.4828336235133043886, 0.000000000000000000 ) ) ;
#23989 = VERTEX_POINT ( 'NONE', #12562 ) ;
#23990 = ORIENTED_EDGE ( 'NONE', *, *, #15507, .T. ) ;
#23991 = LINE ( 'NONE', #14934, #1380 ) ;
#23992 = CARTESIAN_POINT ( 'NONE',  ( -6.233975306307046963E-13, 9.127583699786111282, -11.13316557810918894 ) ) ;
#23993 = CIRCLE ( 'NONE', #18545, 4.172000000000008590 ) ;
#23994 = AXIS2_PLACEMENT_3D ( 'NONE', #21602, #5237, #3160 ) ;
#23995 = CIRCLE ( 'NONE', #19340, 4.172000000000008590 ) ;
#23996 = LINE ( 'NONE', #14713, #9106 ) ;
#23997 = CARTESIAN_POINT ( 'NONE',  ( 18.50000000000000000, 15.23000000000000398, 27.00000000000000000 ) ) ;
#23998 = DIRECTION ( 'NONE',  ( 0.000000000000000000, 0.000000000000000000, 1.000000000000000000 ) ) ;
#23999 = LINE ( 'NONE', #3858, #2911 ) ;
#24000 = FACE_OUTER_BOUND ( 'NONE', #9431, .T. ) ;
#24001 = AXIS2_PLACEMENT_3D ( 'NONE', #23375, #17743, #1045 ) ;
#24002 = LINE ( 'NONE', #9224, #9057 ) ;
#24003 = ORIENTED_EDGE ( 'NONE', *, *, #13907, .F. ) ;
#24004 = EDGE_CURVE ( 'NONE', #3425, #10554, #17960, .T. ) ;
#24005 = ORIENTED_EDGE ( 'NONE', *, *, #8474, .T. ) ;
#24006 = DIRECTION ( 'NONE',  ( 0.000000000000000000, -0.000000000000000000, 1.000000000000000000 ) ) ;
#24007 = CARTESIAN_POINT ( 'NONE',  ( 40.29291594121673370, -26.62062637246459573, 11.00000000000000000 ) ) ;
#24008 = LINE ( 'NONE', #11042, #7095 ) ;
#24009 = EDGE_CURVE ( 'NONE', #704, #18466, #7651, .T. ) ;
#24010 = DIRECTION ( 'NONE',  ( 0.000000000000000000, 1.000000000000000000, 0.000000000000000000 ) ) ;
#24011 = DIRECTION ( 'NONE',  ( -1.000000000000000000, -1.224606353822377258E-16, -0.000000000000000000 ) ) ;
#24012 = VECTOR ( 'NONE', #11388, 1000.000000000000000 ) ;
#24013 = ADVANCED_FACE ( 'NONE', ( #3435, #14517, #16597, #16245, #7205, #24046, #3316, #14168 ), #22119, .F. ) ;
#24014 = AXIS2_PLACEMENT_3D ( 'NONE', #19622, #19856, #17786 ) ;
#24015 = ORIENTED_EDGE ( 'NONE', *, *, #19415, .T. ) ;
#24016 = AXIS2_PLACEMENT_3D ( 'NONE', #23131, #6540, #17499 ) ;
#24017 = ORIENTED_EDGE ( 'NONE', *, *, #19394, .F. ) ;
#24018 = CARTESIAN_POINT ( 'NONE',  ( -6.822232771736903637E-13, 9.988891130263535700, 7.706742014460232326 ) ) ;
#24019 = ORIENTED_EDGE ( 'NONE', *, *, #15206, .F. ) ;
#24020 = ORIENTED_EDGE ( 'NONE', *, *, #7300, .F. ) ;
#24021 = SHAPE_REPRESENTATION_RELATIONSHIP ( 'NONE' , 'NONE' ,  #15960, #18615 ) ;
#24022 = CIRCLE ( 'NONE', #17795, 1.999999999999994449 ) ;
#24023 = COLOUR_RGB ( '',0.7921568627450980005, 0.8196078431372548767, 0.9333333333333333481 ) ;
#24024 = CARTESIAN_POINT ( 'NONE',  ( 9.500000000000000000, 6.470877716354879437E-13, -5.206742014460234103 ) ) ;
#24025 = DIRECTION ( 'NONE',  ( 1.000000000000000000, 1.224606353822377258E-16, 0.000000000000000000 ) ) ;
#24026 = CARTESIAN_POINT ( 'NONE',  ( 83.30704456891035647, 7.562528597612068045E-15, 0.000000000000000000 ) ) ;
#24027 = DIRECTION ( 'NONE',  ( -1.000000000000000000, 0.000000000000000000, 0.000000000000000000 ) ) ;
#24028 = ADVANCED_FACE ( 'NONE', ( #10850 ), #22117, .F. ) ;
#24029 = VECTOR ( 'NONE', #4059, 1000.000000000000000 ) ;
#24030 = ORIENTED_EDGE ( 'NONE', *, *, #6346, .T. ) ;
#24031 = CIRCLE ( 'NONE', #7987, 6.050000000006050982 ) ;
#24032 = EDGE_CURVE ( 'NONE', #21975, #14074, #23585, .T. ) ;
#24033 = CARTESIAN_POINT ( 'NONE',  ( 87.67068093254673045, 6.123233995736675563E-16, -5.000000000000007994 ) ) ;
#24034 = FACE_OUTER_BOUND ( 'NONE', #23816, .T. ) ;
#24035 = DIRECTION ( 'NONE',  ( 0.000000000000000000, 0.000000000000000000, -1.000000000000000000 ) ) ;
#24036 = DIRECTION ( 'NONE',  ( -1.000000000000000000, -1.224606353822377258E-16, -0.000000000000000000 ) ) ;
#24037 = VECTOR ( 'NONE', #8409, 1000.000000000000000 ) ;
#24038 = EDGE_CURVE ( 'NONE', #19120, #13598, #14289, .T. ) ;
#24039 = DIRECTION ( 'NONE',  ( -0.000000000000000000, -1.000000000000000000, -0.000000000000000000 ) ) ;
#24040 = CARTESIAN_POINT ( 'NONE',  ( 21.13207267780287069, 38.32709852940855910, 12.00000000000000000 ) ) ;
#24041 = ORIENTED_EDGE ( 'NONE', *, *, #7694, .T. ) ;
#24042 = LINE ( 'NONE', #16808, #2534 ) ;
#24043 = ORIENTED_EDGE ( 'NONE', *, *, #17919, .T. ) ;
#24044 = CARTESIAN_POINT ( 'NONE',  ( -5.871322893123449127, -8.081182679344781405, -9.359589141758144493 ) ) ;
#24045 = VERTEX_POINT ( 'NONE', #8910 ) ;
#24046 = FACE_BOUND ( 'NONE', #15796, .T. ) ;
#24047 = AXIS2_PLACEMENT_3D ( 'NONE', #15328, #461, #23939 ) ;
#24048 = LINE ( 'NONE', #12923, #10667 ) ;
#24049 = DIRECTION ( 'NONE',  ( 0.000000000000000000, 0.000000000000000000, 1.000000000000000000 ) ) ;
#24050 = CARTESIAN_POINT ( 'NONE',  ( -14.51962751333974033, -3.765689428759031010, 8.721787840009202597 ) ) ;
#24051 = CARTESIAN_POINT ( 'NONE',  ( -5.871322893124554021, 8.081182679343978492, -4.759589141758144848 ) ) ;
#24052 = ORIENTED_EDGE ( 'NONE', *, *, #2179, .F. ) ;
#24053 = ORIENTED_EDGE ( 'NONE', *, *, #18967, .F. ) ;
#24054 = CARTESIAN_POINT ( 'NONE',  ( 0.000000000000000000, 0.000000000000000000, 105.0000000000000000 ) ) ;
#24055 = CARTESIAN_POINT ( 'NONE',  ( 27.89784171216406961, 41.49349862090490859, -1.500000000000000000 ) ) ;
#24056 = EDGE_CURVE ( 'NONE', #15133, #12531, #17825, .T. ) ;
#24057 = EDGE_CURVE ( 'NONE', #9249, #23971, #5343, .T. ) ;
#24058 = VERTEX_POINT ( 'NONE', #7077 ) ;
#24059 = ORIENTED_EDGE ( 'NONE', *, *, #20204, .T. ) ;
#24060 = LINE ( 'NONE', #7338, #19615 ) ;
#24061 = CARTESIAN_POINT ( 'NONE',  ( -1.999999999999994449, -45.00000000000000000, 23.99999999999999645 ) ) ;
#24062 = ORIENTED_EDGE ( 'NONE', *, *, #17125, .F. ) ;
#24063 = CARTESIAN_POINT ( 'NONE',  ( 0.000000000000000000, -45.00000000000000000, -27.00000000000000000 ) ) ;
#24064 = DIRECTION ( 'NONE',  ( -1.000000000000000000, 0.000000000000000000, 0.000000000000000000 ) ) ;
#24065 = FACE_OUTER_BOUND ( 'NONE', #10874, .T. ) ;
#24066 = FACE_OUTER_BOUND ( 'NONE', #15141, .T. ) ;
#24067 = ORIENTED_EDGE ( 'NONE', *, *, #268, .F. ) ;
#24068 = ORIENTED_EDGE ( 'NONE', *, *, #12853, .T. ) ;
#24069 = ORIENTED_EDGE ( 'NONE', *, *, #4791, .F. ) ;
#24070 = EDGE_CURVE ( 'NONE', #9582, #1469, #19805, .T. ) ;
#24071 = ORIENTED_EDGE ( 'NONE', *, *, #16187, .F. ) ;
#24072 = ORIENTED_EDGE ( 'NONE', *, *, #2073, .T. ) ;
#24073 = CARTESIAN_POINT ( 'NONE',  ( -6.250000000000000888, 10.82531754730548279, 2.500000000000000000 ) ) ;
#24074 = EDGE_CURVE ( 'NONE', #16852, #566, #11943, .T. ) ;
#24075 = DIRECTION ( 'NONE',  ( 0.000000000000000000, -0.2817325568414365544, 0.9594929736144953702 ) ) ;
#24076 = EDGE_LOOP ( 'NONE', ( #18833, #746, #9091, #23650 ) ) ;
#24077 = EDGE_CURVE ( 'NONE', #20652, #8837, #1072, .T. ) ;
#24078 = EDGE_CURVE ( 'NONE', #3028, #19491, #11357, .T. ) ;
#24079 = EDGE_CURVE ( 'NONE', #12610, #9321, #17011, .T. ) ;
#24080 = CARTESIAN_POINT ( 'NONE',  ( 40.23082370883257397, -29.49999999999999645, -3.000000000000000000 ) ) ;
#24081 = EDGE_LOOP ( 'NONE', ( #876, #22549, #6620, #23901 ) ) ;
#24082 = CARTESIAN_POINT ( 'NONE',  ( 0.000000000000000000, 45.00000000000000000, -8.673617379884035472E-16 ) ) ;
#24083 = DIRECTION ( 'NONE',  ( -1.000000000000000000, 0.000000000000000000, 0.000000000000000000 ) ) ;
#24084 = FACE_OUTER_BOUND ( 'NONE', #14368, .T. ) ;
#24085 = CIRCLE ( 'NONE', #16688, 1.999999999999994449 ) ;
#24086 = DIRECTION ( 'NONE',  ( 1.000000000000000000, 0.000000000000000000, 0.000000000000000000 ) ) ;
#24087 = DIRECTION ( 'NONE',  ( 0.000000000000000000, 0.000000000000000000, 1.000000000000000000 ) ) ;
#24088 = PRESENTATION_LAYER_ASSIGNMENT (  '', '', ( #20203 ) ) ;
#24089 = CARTESIAN_POINT ( 'NONE',  ( 79.81818181818181301, 4.172000000000015696, 5.109226446042767468E-16 ) ) ;
#24090 = CARTESIAN_POINT ( 'NONE',  ( 42.00000000000000000, -26.82133436441678853, 11.00000000000000000 ) ) ;
#24091 = DIRECTION ( 'NONE',  ( 0.000000000000000000, 0.000000000000000000, -1.000000000000000000 ) ) ;
#24092 = DIRECTION ( 'NONE',  ( -0.5735764363510517105, -0.8191520442889879128, 0.000000000000000000 ) ) ;
#24093 = ORIENTED_EDGE ( 'NONE', *, *, #3438, .T. ) ;
#24094 = CARTESIAN_POINT ( 'NONE',  ( -8.680847955711007202, -5.923547351154968927E-13, 9.633165578109188942 ) ) ;
#24095 = ORIENTED_EDGE ( 'NONE', *, *, #8497, .F. ) ;
#24096 = APPLICATION_PROTOCOL_DEFINITION ( 'draft international standard', 'automotive_design', 1998, #16939 ) ;
#24097 = EDGE_CURVE ( 'NONE', #19436, #671, #18086, .T. ) ;
#24098 = CARTESIAN_POINT ( 'NONE',  ( 0.000000000000000000, 0.000000000000000000, 14.72592346043842326 ) ) ;
#24099 = NEXT_ASSEMBLY_USAGE_OCCURRENCE ( 'NAUO1', ' ', ' ', #5009, #12281, $ ) ;
#24100 = NEXT_ASSEMBLY_USAGE_OCCURRENCE ( 'NAUO2', ' ', ' ', #5009, #16898, $ ) ;
#24101 = NEXT_ASSEMBLY_USAGE_OCCURRENCE ( 'NAUO3', ' ', ' ', #5009, #16898, $ ) ;
#24102 = NEXT_ASSEMBLY_USAGE_OCCURRENCE ( 'NAUO4', ' ', ' ', #5009, #8241, $ ) ;
#24103 = NEXT_ASSEMBLY_USAGE_OCCURRENCE ( 'NAUO5', ' ', ' ', #5009, #13774, $ ) ;
#24104 = NEXT_ASSEMBLY_USAGE_OCCURRENCE ( 'NAUO6', ' ', ' ', #5009, #8694, $ ) ;
#24105 = NEXT_ASSEMBLY_USAGE_OCCURRENCE ( 'NAUO7', ' ', ' ', #5009, #17349, $ ) ;
#24106 = NEXT_ASSEMBLY_USAGE_OCCURRENCE ( 'NAUO8', ' ', ' ', #5009, #13774, $ ) ;
#24107 = NEXT_ASSEMBLY_USAGE_OCCURRENCE ( 'NAUO9', ' ', ' ', #5009, #16898, $ ) ;
#24108 = NEXT_ASSEMBLY_USAGE_OCCURRENCE ( 'NAUO10', ' ', ' ', #5009, #16898, $ ) ;
#24109 = NEXT_ASSEMBLY_USAGE_OCCURRENCE ( 'NAUO11', ' ', ' ', #5009, #1431, $ ) ;
#24110 = NEXT_ASSEMBLY_USAGE_OCCURRENCE ( 'NAUO12', ' ', ' ', #5009, #1431, $ ) ;
#24111 = NEXT_ASSEMBLY_USAGE_OCCURRENCE ( 'NAUO13', ' ', ' ', #5009, #1431, $ ) ;
#24112 = NEXT_ASSEMBLY_USAGE_OCCURRENCE ( 'NAUO14', ' ', ' ', #5009, #1431, $ ) ;
#24113 = NEXT_ASSEMBLY_USAGE_OCCURRENCE ( 'NAUO15', ' ', ' ', #5009, #8989, $ ) ;
#24114 = NEXT_ASSEMBLY_USAGE_OCCURRENCE ( 'NAUO16', ' ', ' ', #5009, #16174, $ ) ;
#24115 = NEXT_ASSEMBLY_USAGE_OCCURRENCE ( 'NAUO17', ' ', ' ', #5009, #16174, $ ) ;
#24116 = NEXT_ASSEMBLY_USAGE_OCCURRENCE ( 'NAUO18', ' ', ' ', #5009, #16174, $ ) ;
#24117 = NEXT_ASSEMBLY_USAGE_OCCURRENCE ( 'NAUO19', ' ', ' ', #5009, #16174, $ ) ;
#24118 = NEXT_ASSEMBLY_USAGE_OCCURRENCE ( 'NAUO20', ' ', ' ', #5009, #12542, $ ) ;
#24119 = NEXT_ASSEMBLY_USAGE_OCCURRENCE ( 'NAUO21', ' ', ' ', #5009, #12542, $ ) ;
#24120 = NEXT_ASSEMBLY_USAGE_OCCURRENCE ( 'NAUO22', ' ', ' ', #5009, #10008, $ ) ;
#24121 = NEXT_ASSEMBLY_USAGE_OCCURRENCE ( 'NAUO23', ' ', ' ', #5009, #13603, $ ) ;
#24122 = NEXT_ASSEMBLY_USAGE_OCCURRENCE ( 'NAUO24', ' ', ' ', #17349, #21247, $ ) ;
#24123 = NEXT_ASSEMBLY_USAGE_OCCURRENCE ( 'NAUO25', ' ', ' ', #17349, #8534, $ ) ;
#24124 = NEXT_ASSEMBLY_USAGE_OCCURRENCE ( 'NAUO26', ' ', ' ', #8694, #22438, $ ) ;
#24125 = NEXT_ASSEMBLY_USAGE_OCCURRENCE ( 'NAUO27', ' ', ' ', #8694, #8534, $ ) ;
#24126 = NEXT_ASSEMBLY_USAGE_OCCURRENCE ( 'NAUO28', ' ', ' ', #16898, #2599, $ ) ;
#24127 = NEXT_ASSEMBLY_USAGE_OCCURRENCE ( 'NAUO29', ' ', ' ', #16898, #13308, $ ) ;
#24128=COLOUR_RGB('Dark Blue',0.08,0.2,0.34);
#24129=FILL_AREA_STYLE_COLOUR('',#24128);
#24130=FILL_AREA_STYLE('',(#24129));
#24131=SURFACE_STYLE_FILL_AREA(#24130);
#24132=SURFACE_SIDE_STYLE('',(#24131));
#24133=SURFACE_STYLE_USAGE(.BOTH.,#24132);
#24134=PRESENTATION_STYLE_ASSIGNMENT((#24133));
#24135=COLOUR_RGB('Light Blue',0.38,0.62,0.78);
#24136=FILL_AREA_STYLE_COLOUR('',#24135);
#24137=FILL_AREA_STYLE('',(#24136));
#24138=SURFACE_STYLE_FILL_AREA(#24137);
#24139=SURFACE_SIDE_STYLE('',(#24138));
#24140=SURFACE_STYLE_USAGE(.BOTH.,#24139);
#24141=PRESENTATION_STYLE_ASSIGNMENT((#24140));
#24142=COLOUR_RGB('Sky Blue',0.24,0.69,0.87);
#24143=FILL_AREA_STYLE_COLOUR('',#24142);
#24144=FILL_AREA_STYLE('',(#24143));
#24145=SURFACE_STYLE_FILL_AREA(#24144);
#24146=SURFACE_SIDE_STYLE('',(#24145));
#24147=SURFACE_STYLE_USAGE(.BOTH.,#24146);
#24148=PRESENTATION_STYLE_ASSIGNMENT((#24147));
#24149=COLOUR_RGB('Grey',0.48,0.52,0.57);
#24150=FILL_AREA_STYLE_COLOUR('',#24149);
#24151=FILL_AREA_STYLE('',(#24150));
#24152=SURFACE_STYLE_FILL_AREA(#24151);
#24153=SURFACE_SIDE_STYLE('',(#24152));
#24154=SURFACE_STYLE_USAGE(.BOTH.,#24153);
#24155=PRESENTATION_STYLE_ASSIGNMENT((#24154));
#24156=COLOUR_RGB('Black',0.12,0.14,0.17);
#24157=FILL_AREA_STYLE_COLOUR('',#24156);
#24158=FILL_AREA_STYLE('',(#24157));
#24159=SURFACE_STYLE_FILL_AREA(#24158);
#24160=SURFACE_SIDE_STYLE('',(#24159));
#24161=SURFACE_STYLE_USAGE(.BOTH.,#24160);
#24162=PRESENTATION_STYLE_ASSIGNMENT((#24161));
#24163=COLOUR_RGB('Off White',0.89,0.88,0.83);
#24164=FILL_AREA_STYLE_COLOUR('',#24163);
#24165=FILL_AREA_STYLE('',(#24164));
#24166=SURFACE_STYLE_FILL_AREA(#24165);
#24167=SURFACE_SIDE_STYLE('',(#24166));
#24168=SURFACE_STYLE_USAGE(.BOTH.,#24167);
#24169=PRESENTATION_STYLE_ASSIGNMENT((#24168));
ENDSEC;
END-ISO-10303-21;
